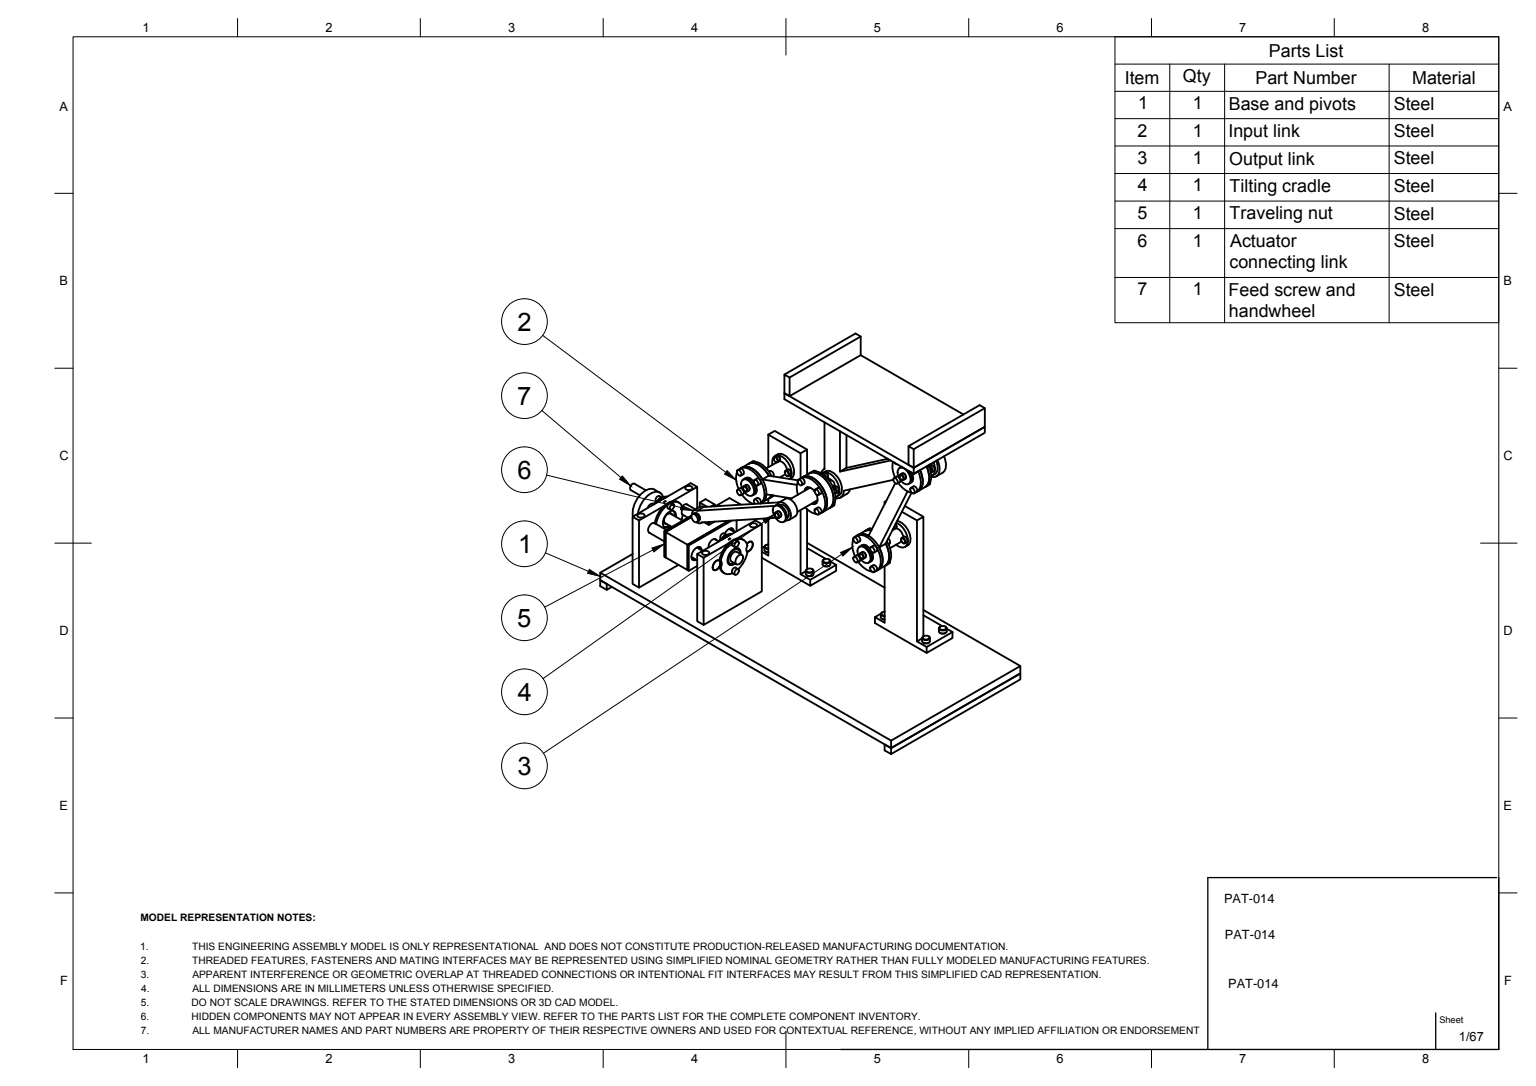
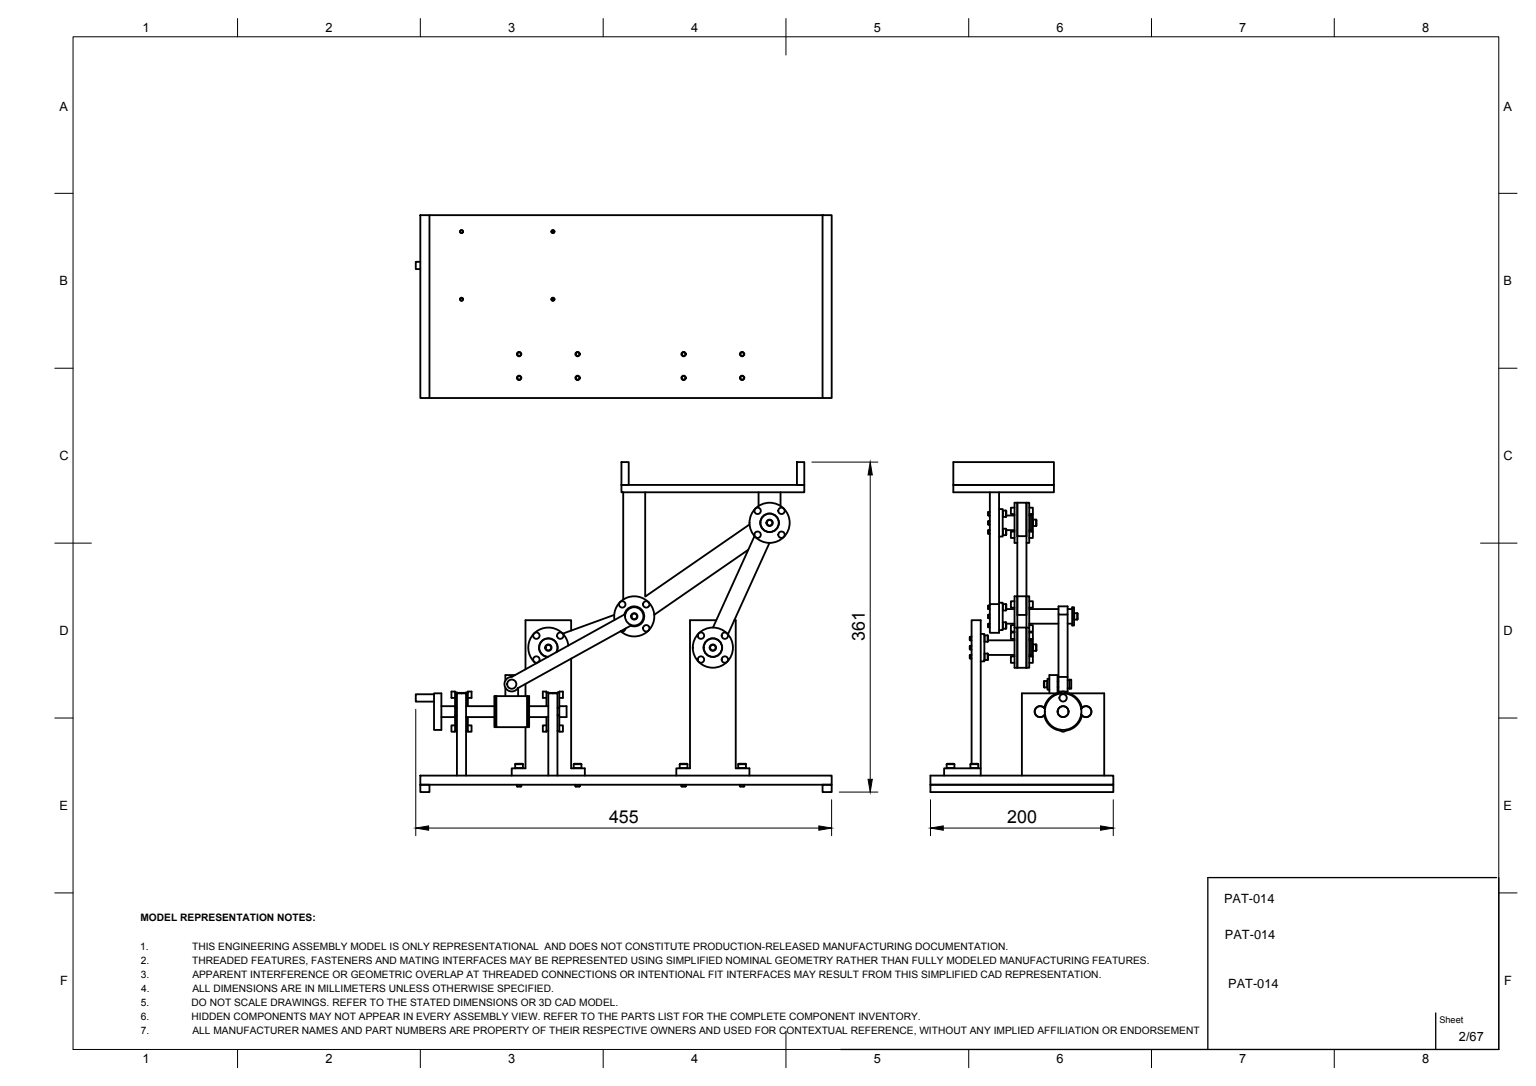
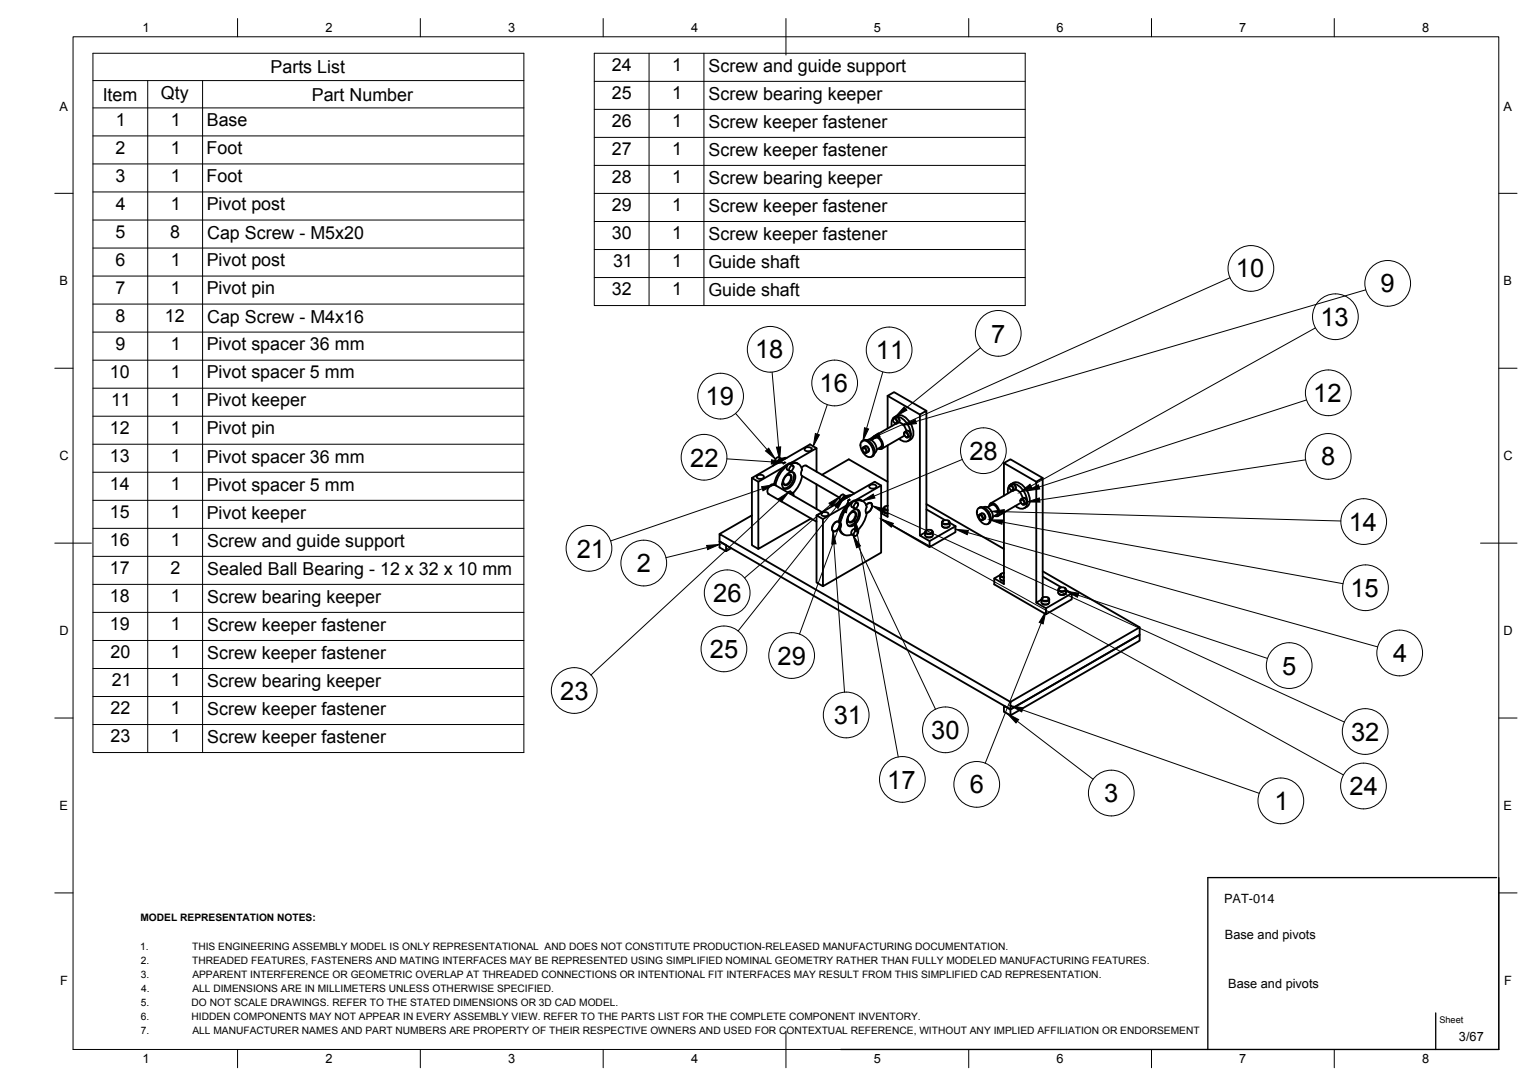
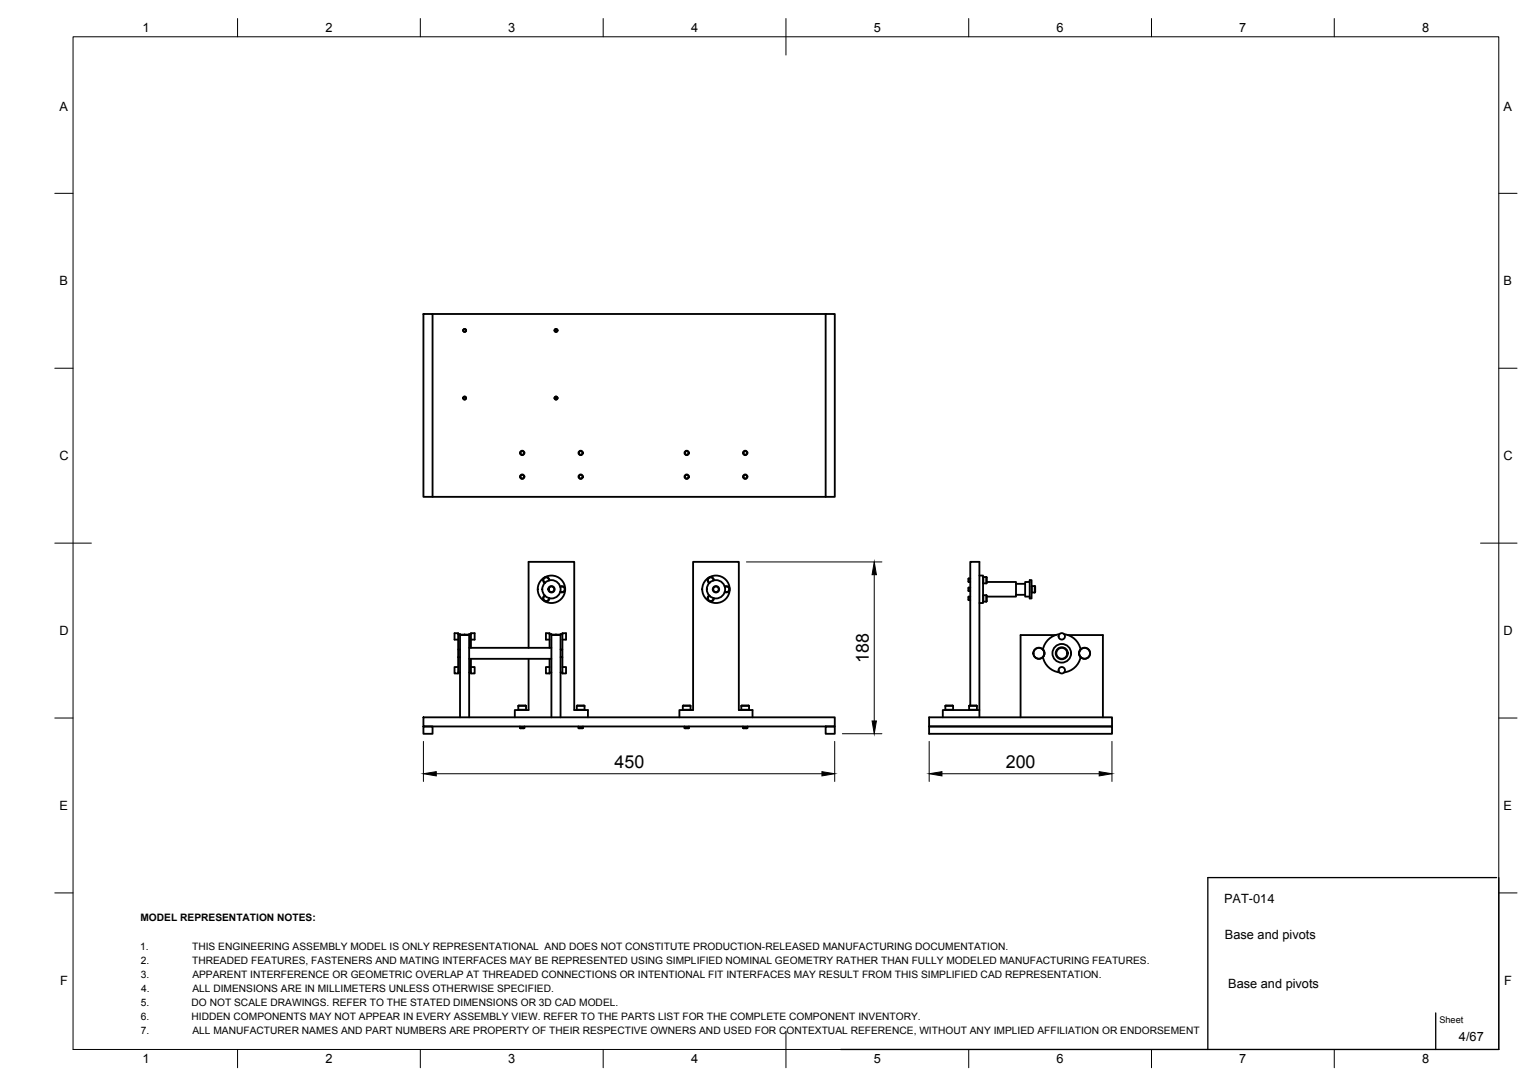
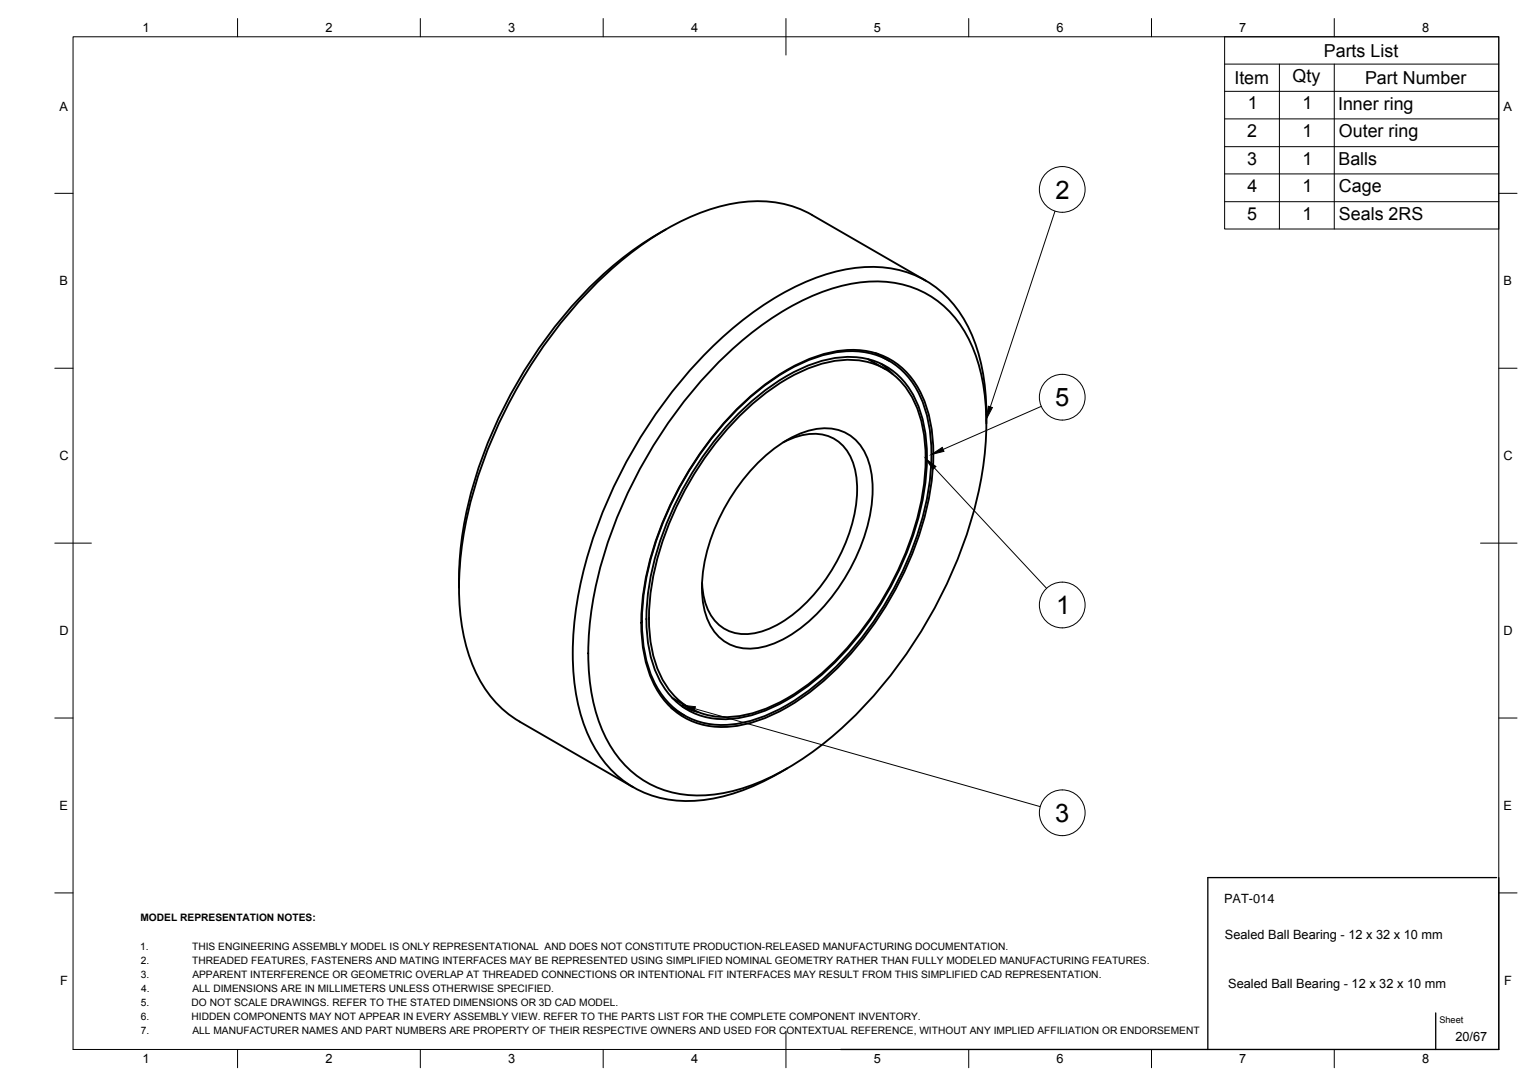
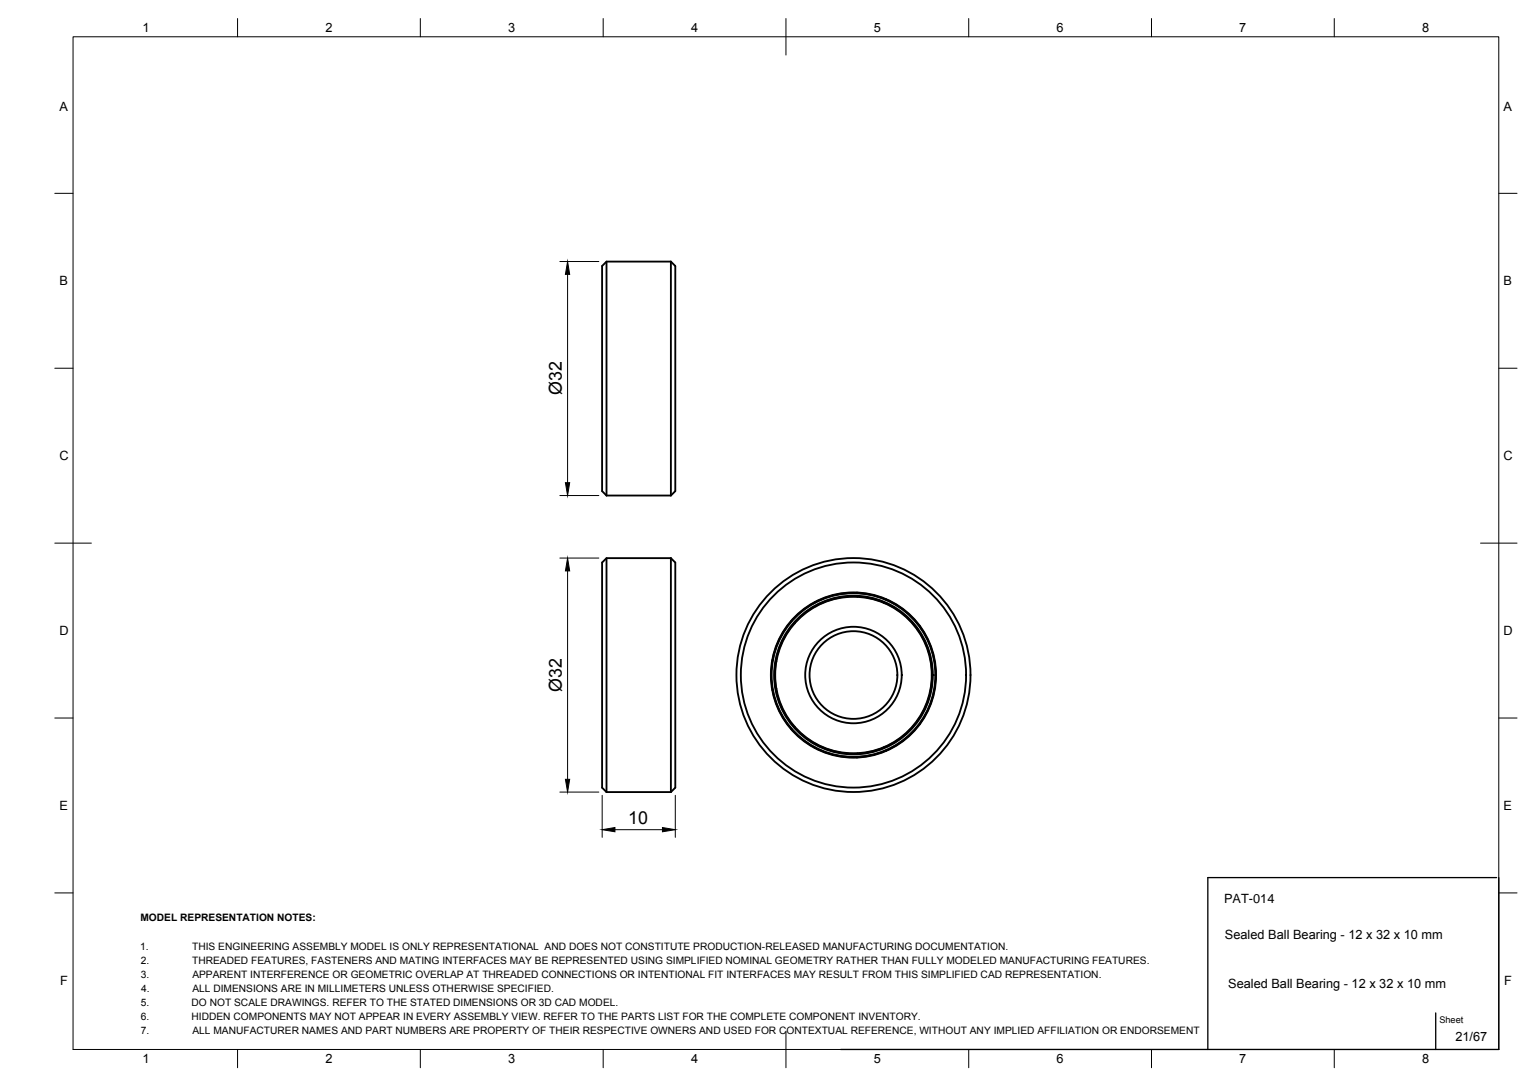
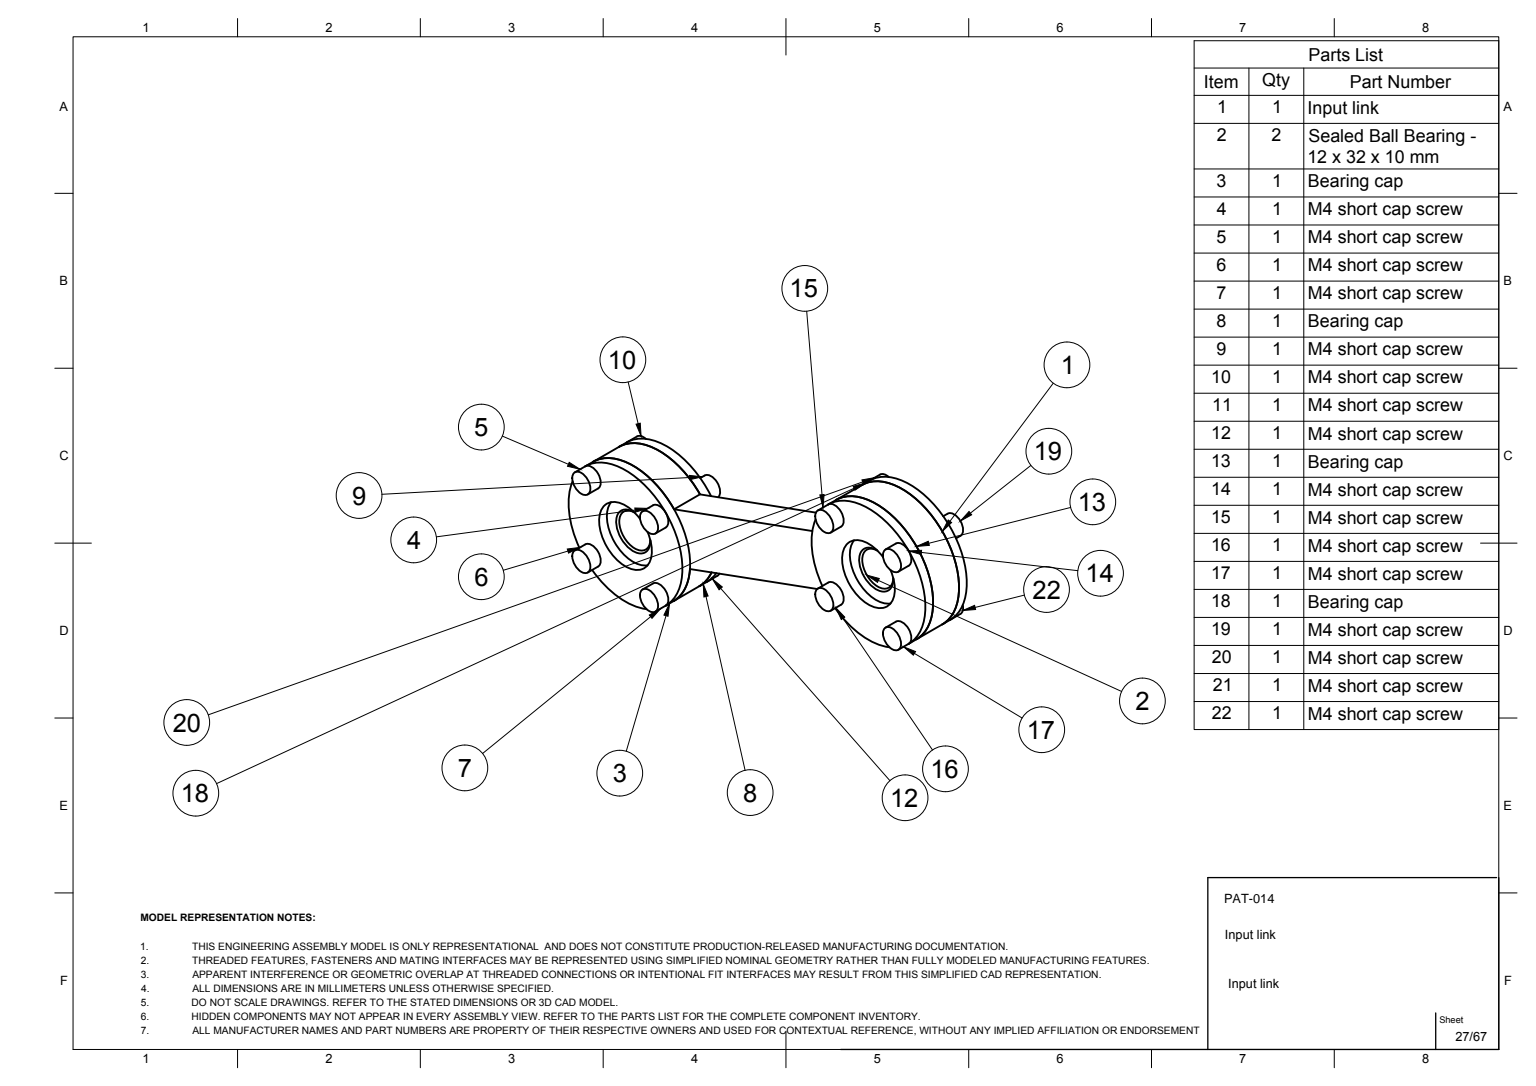
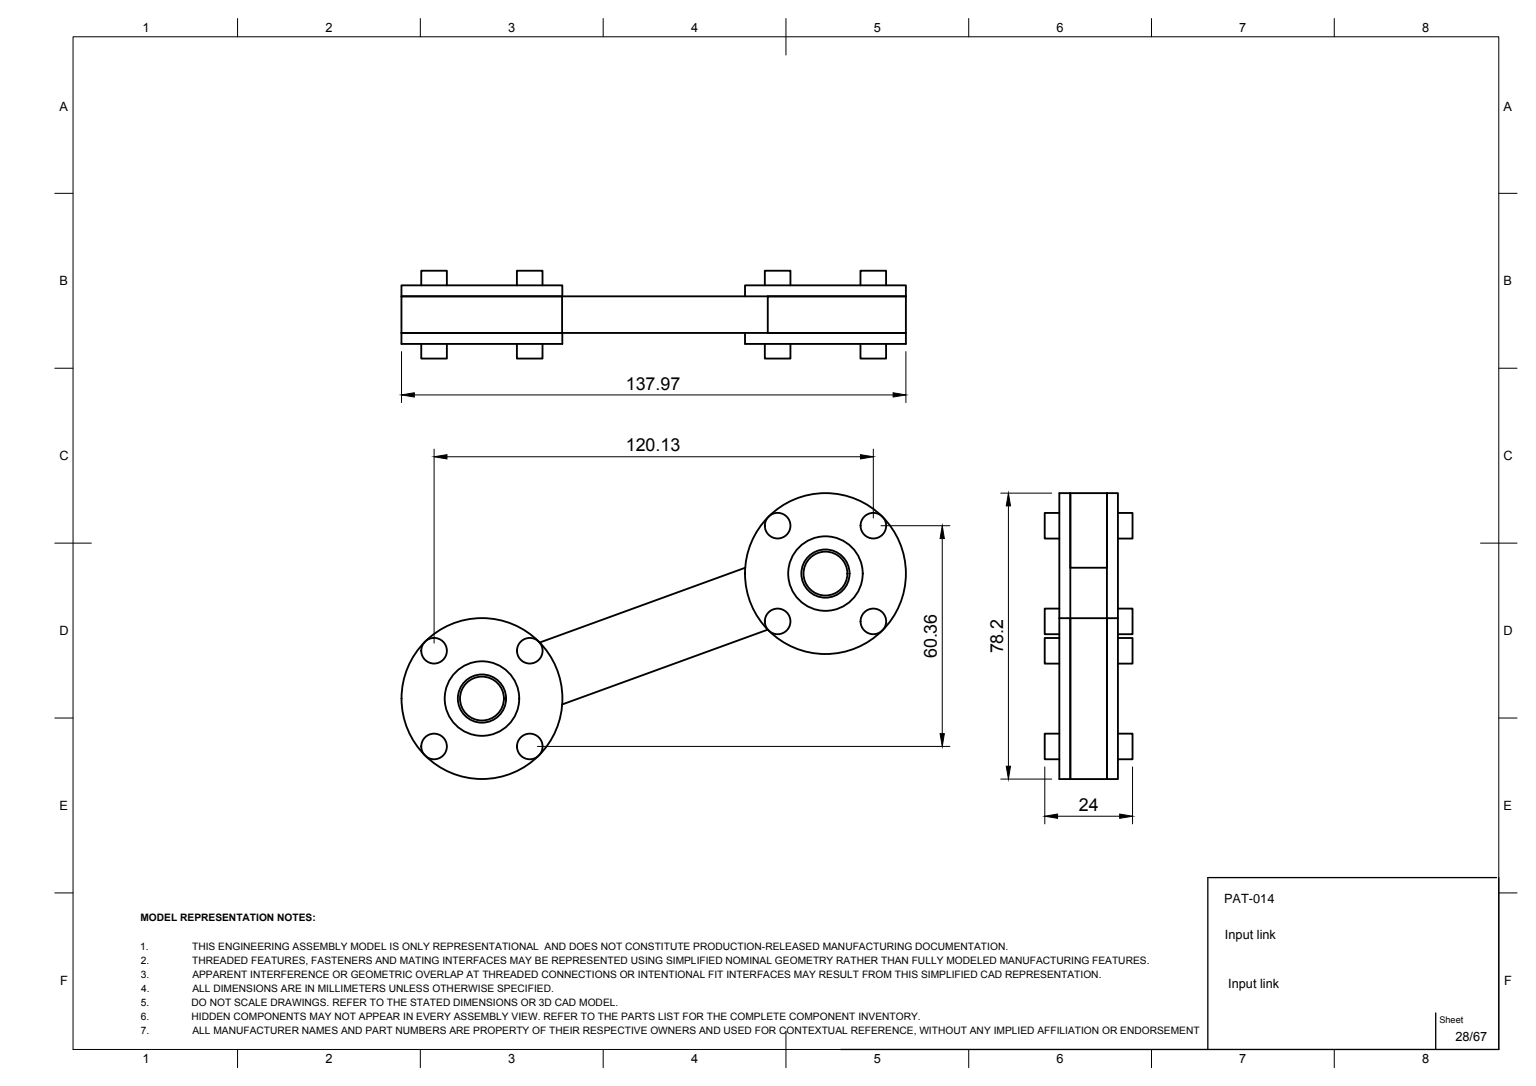
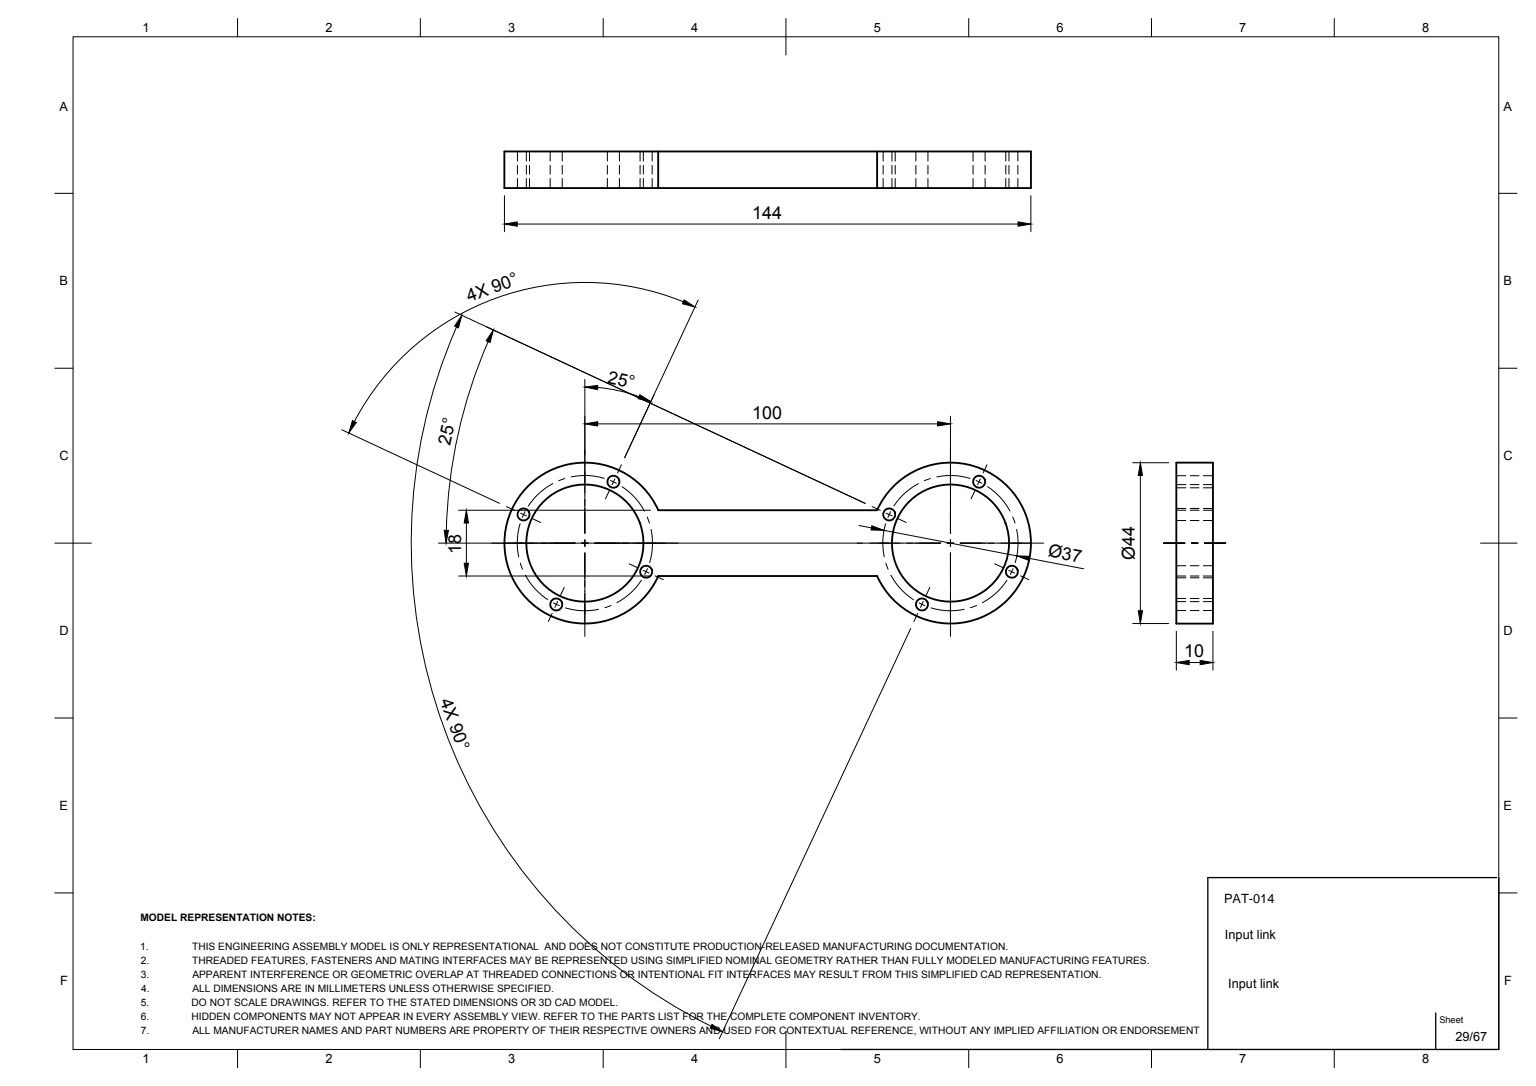
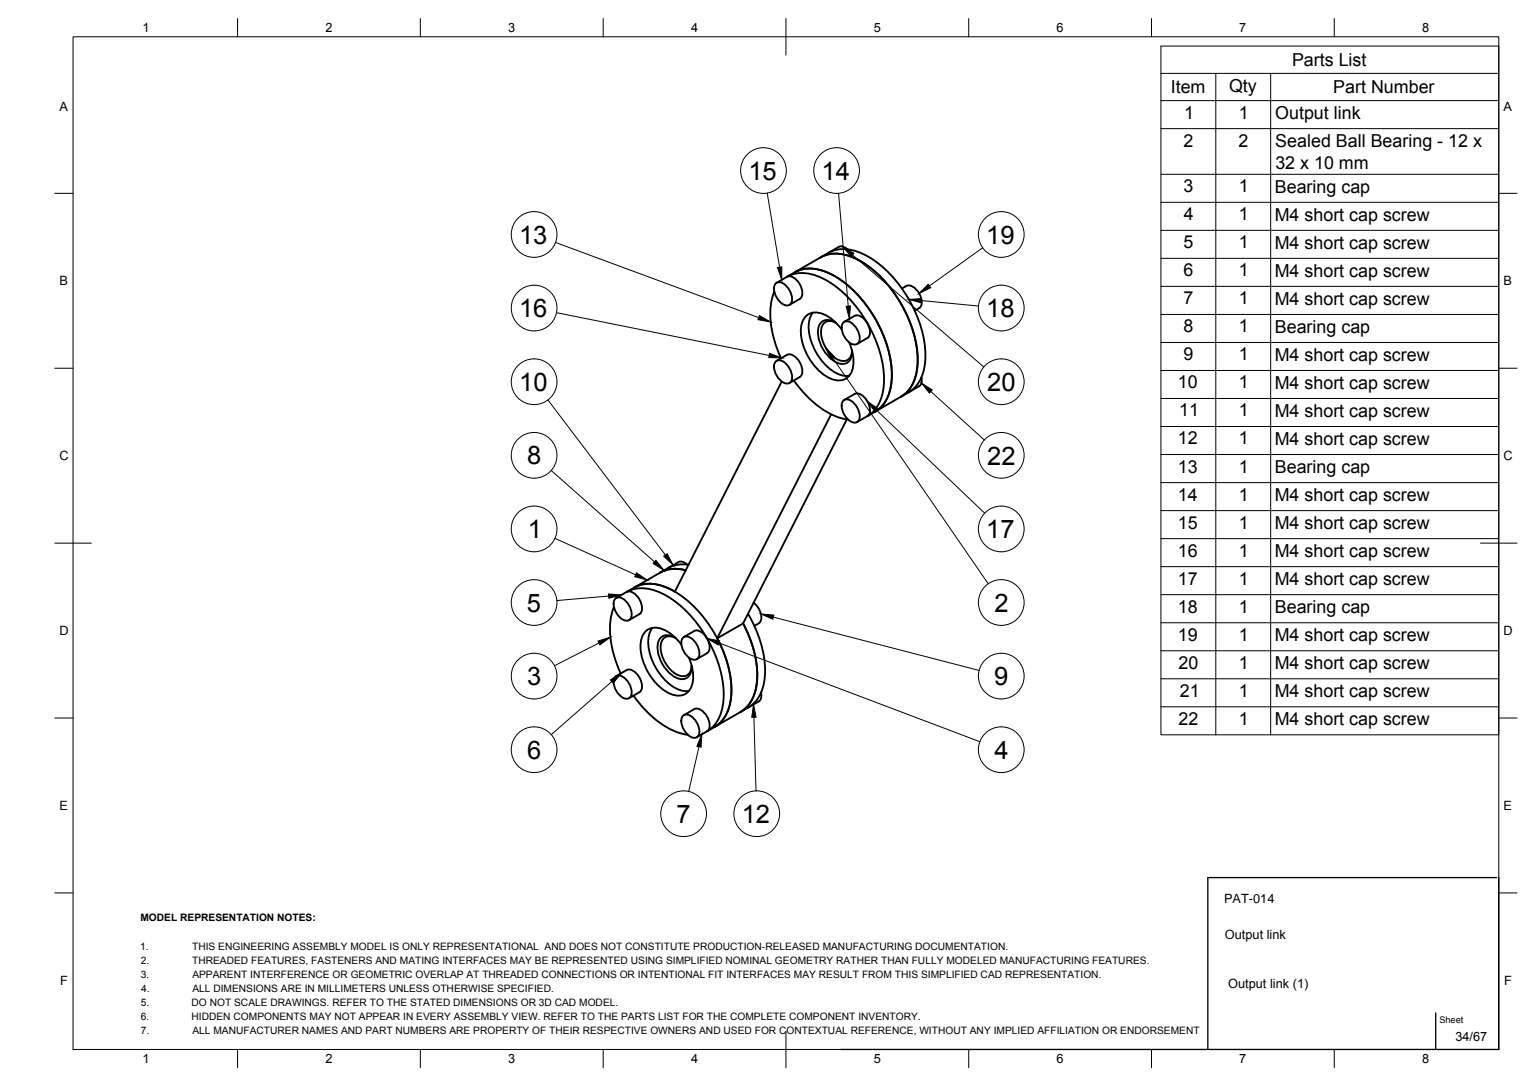
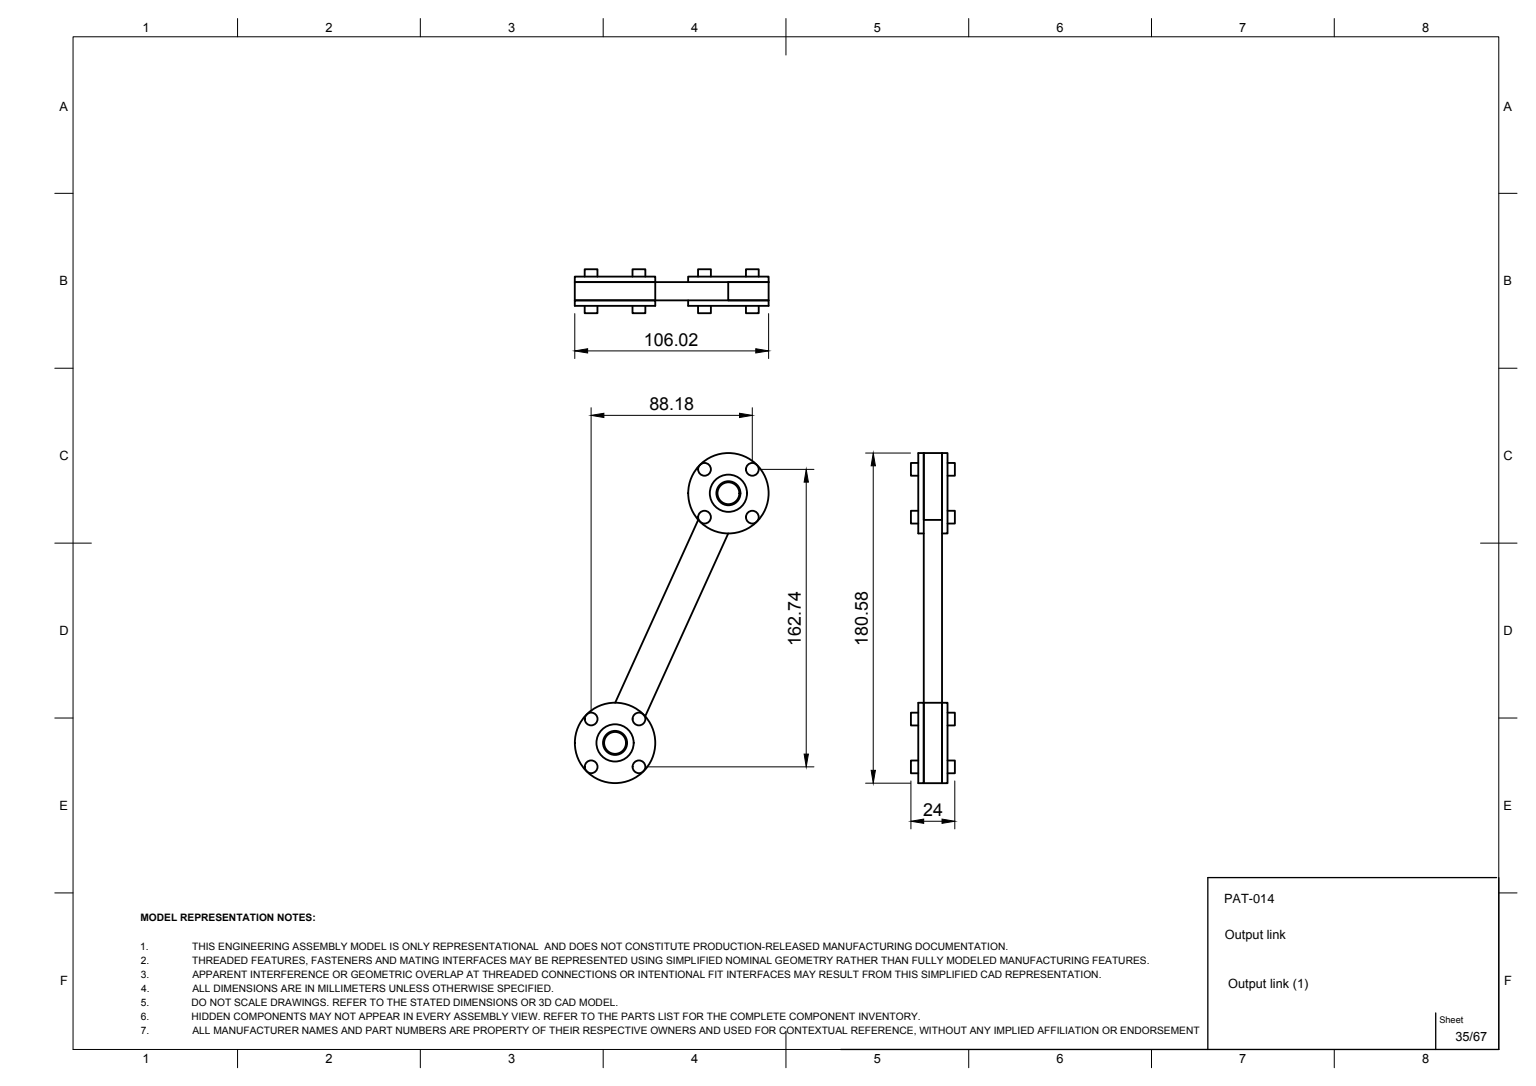
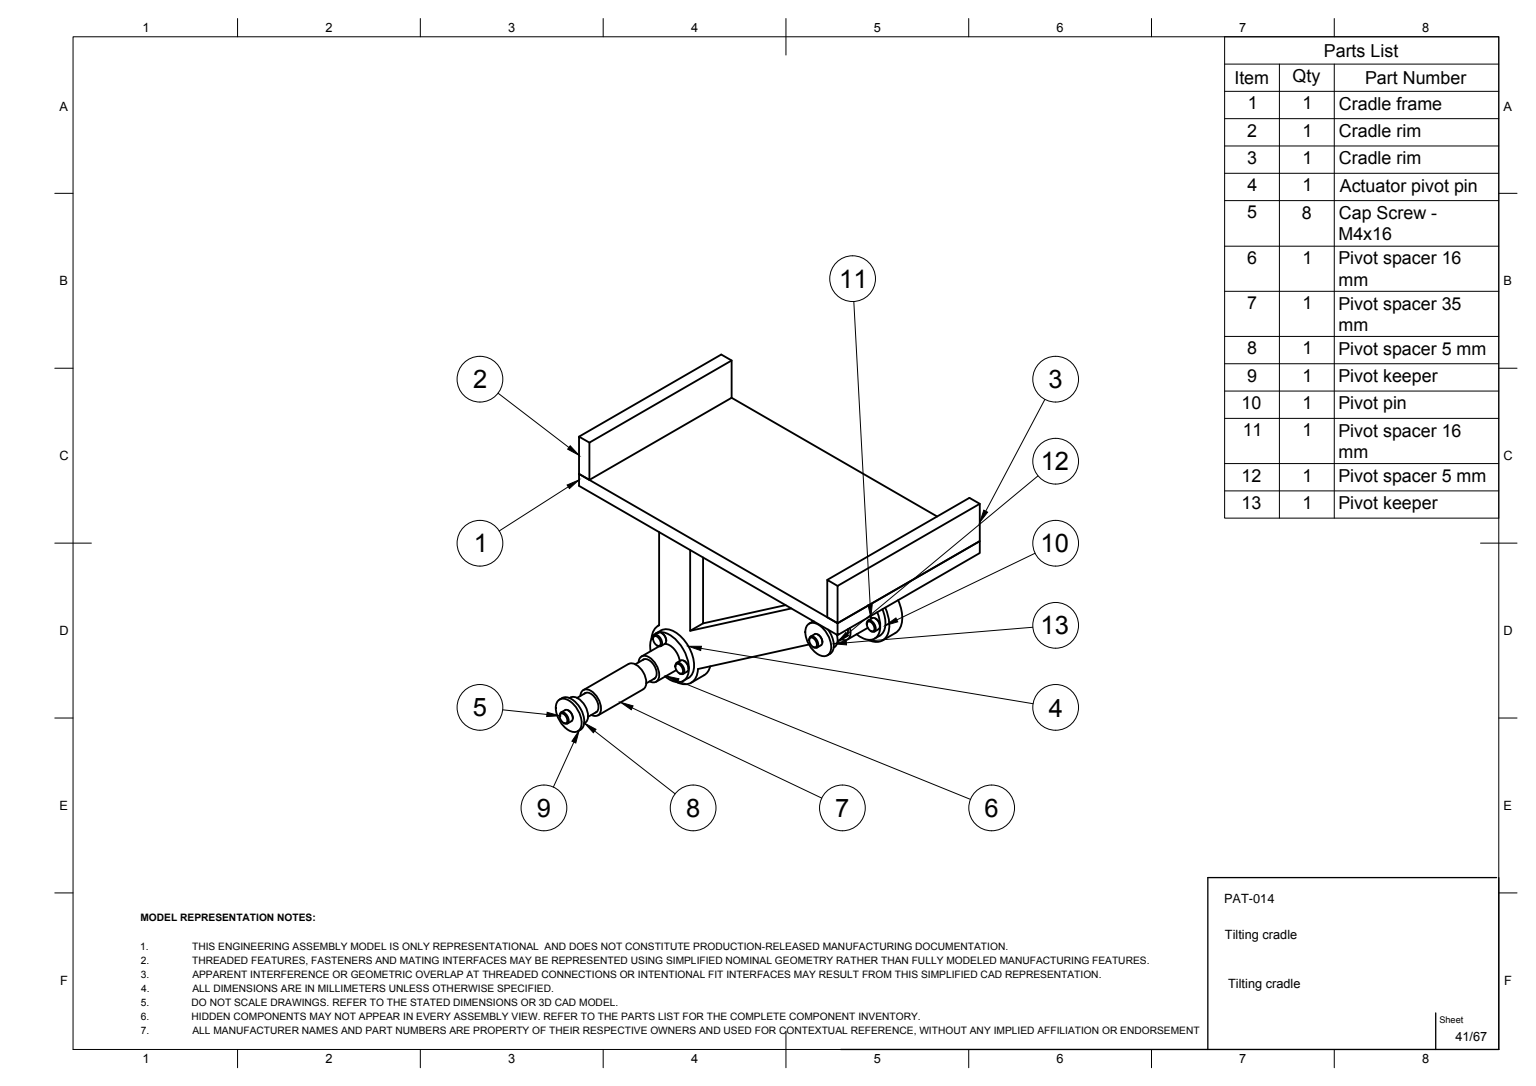
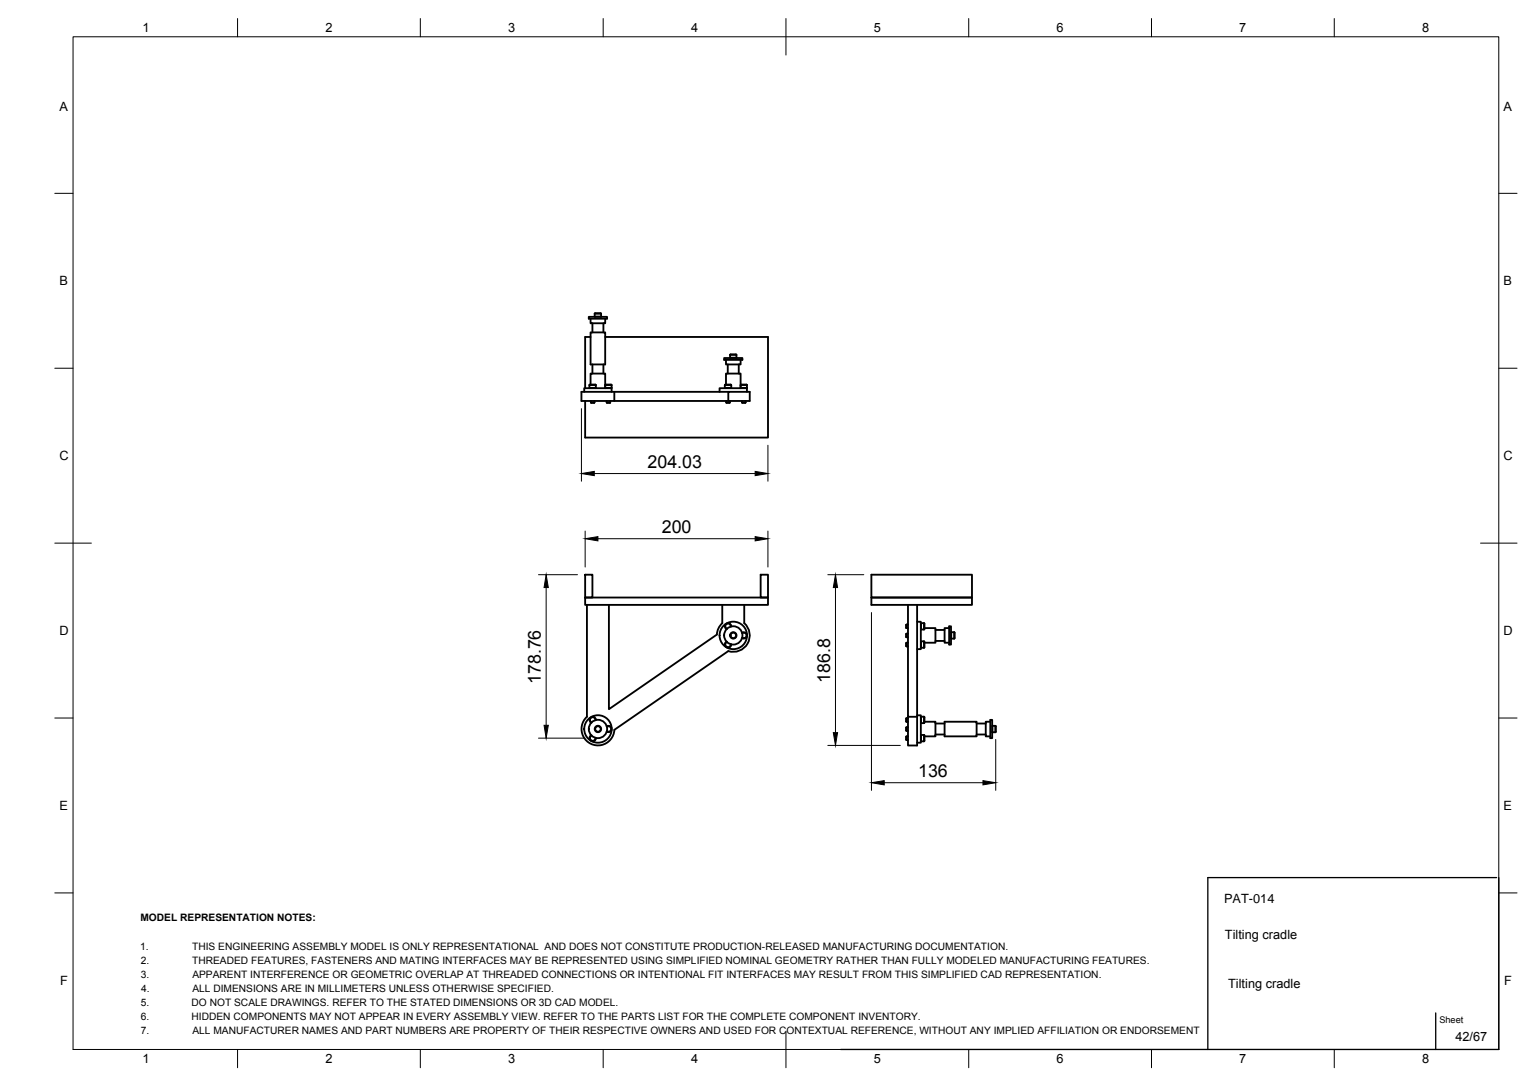
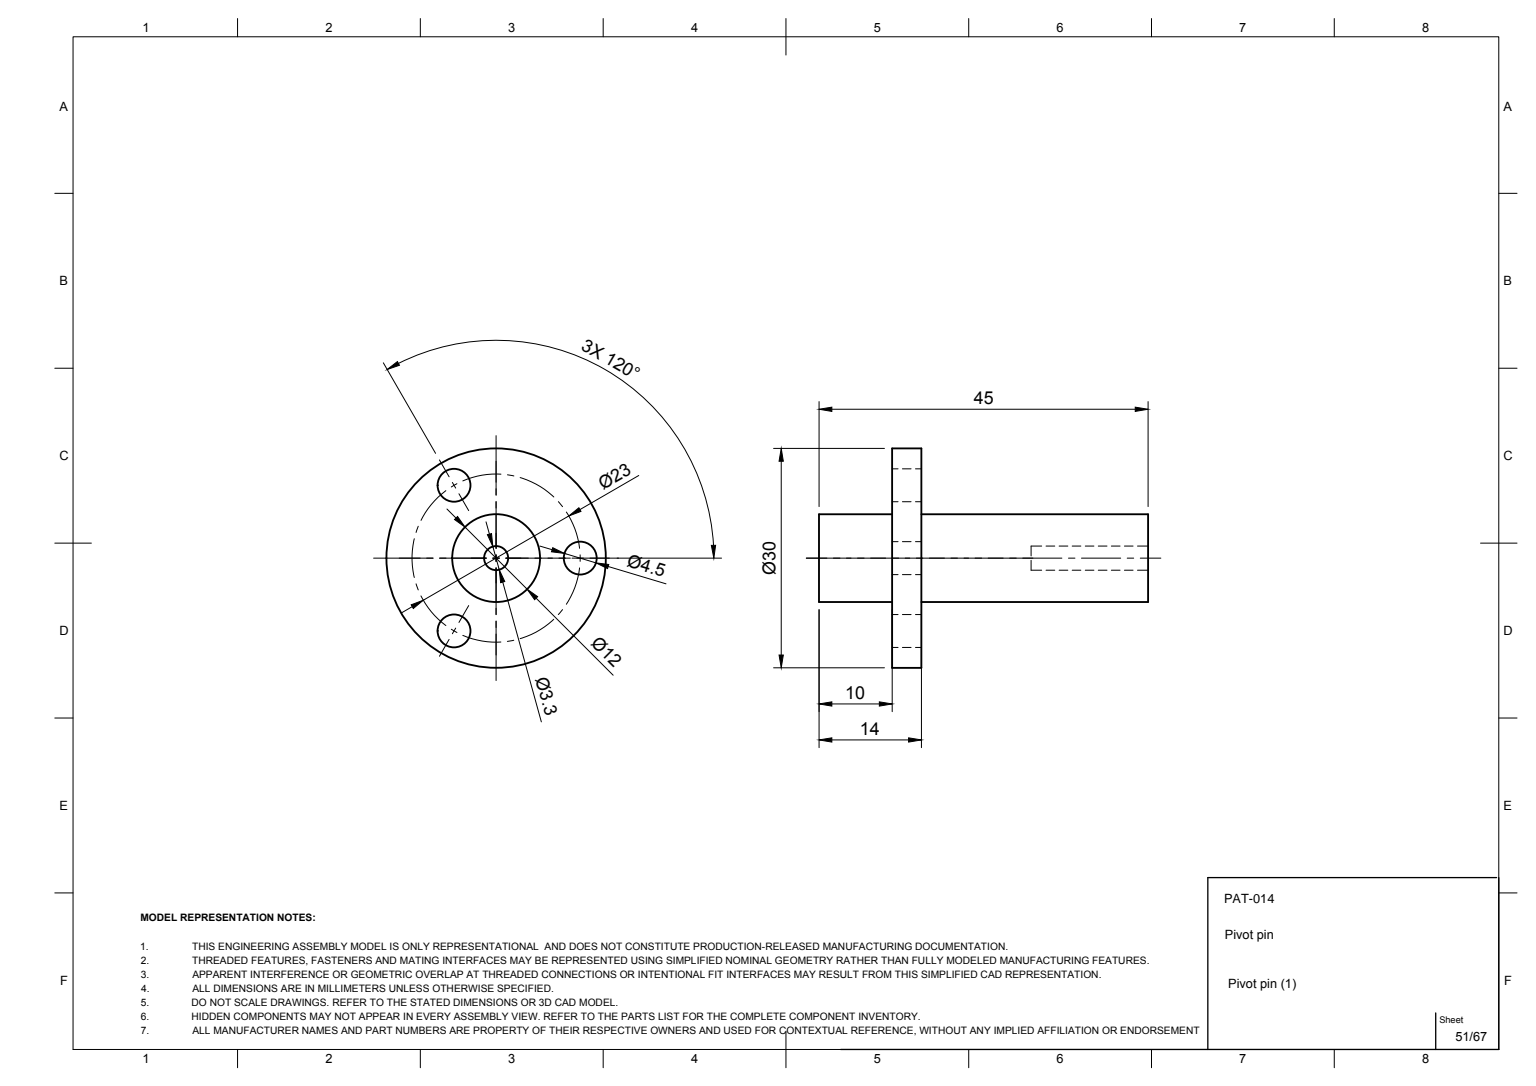
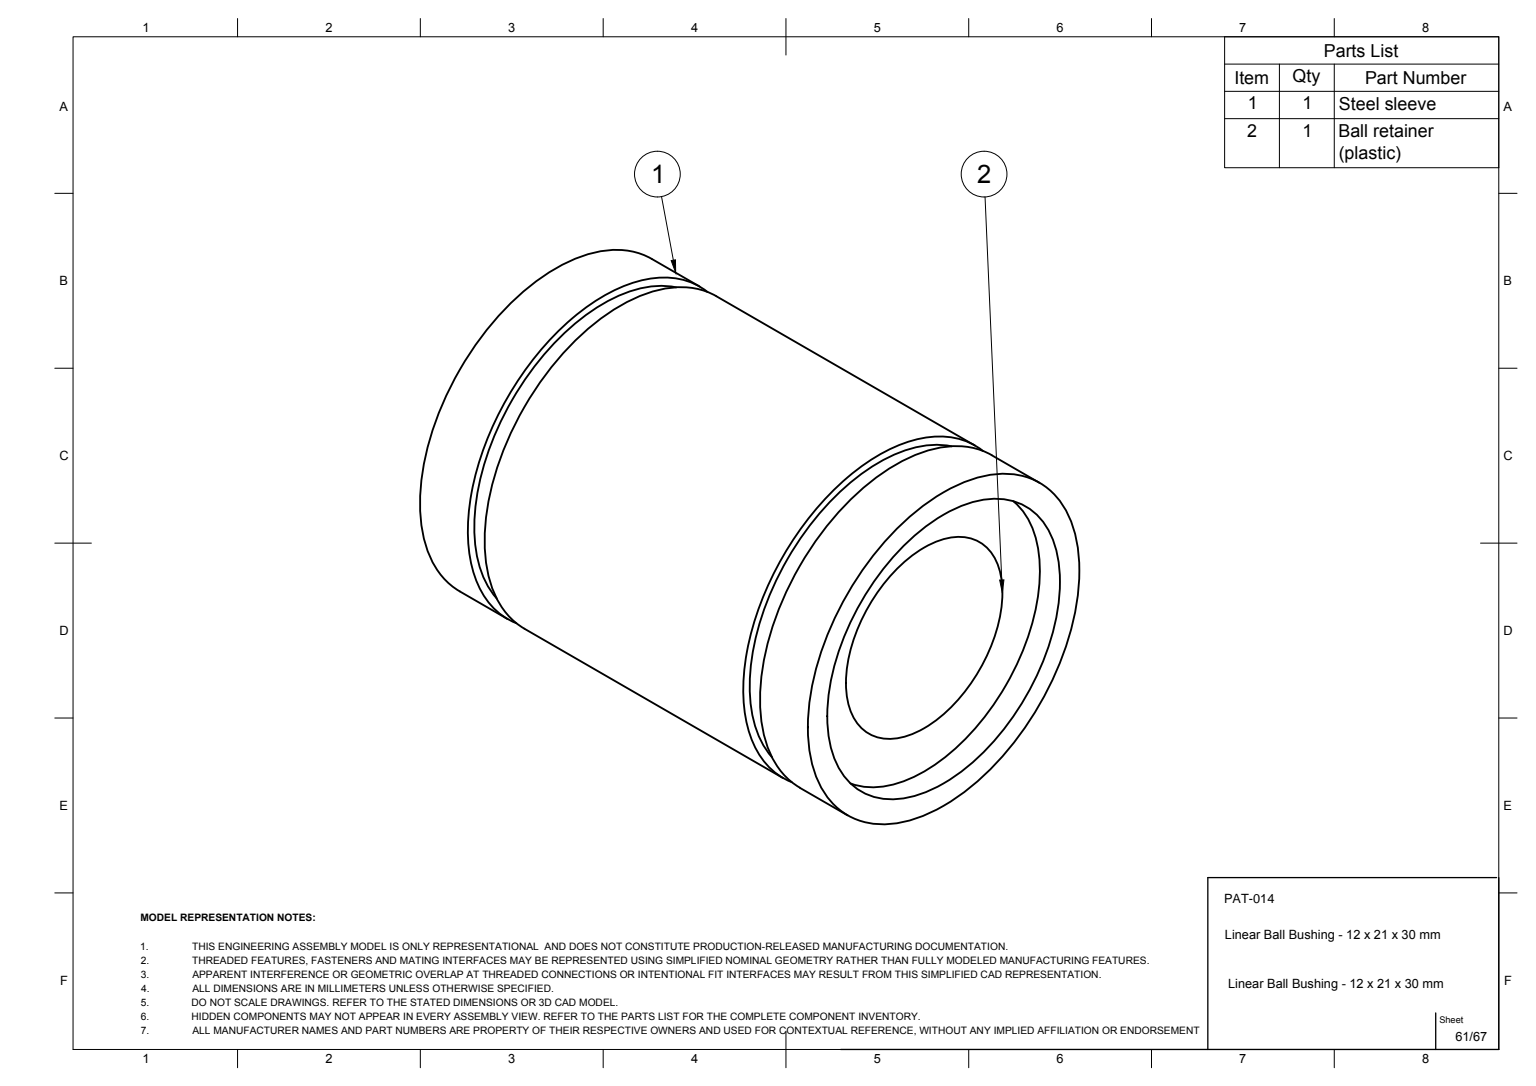
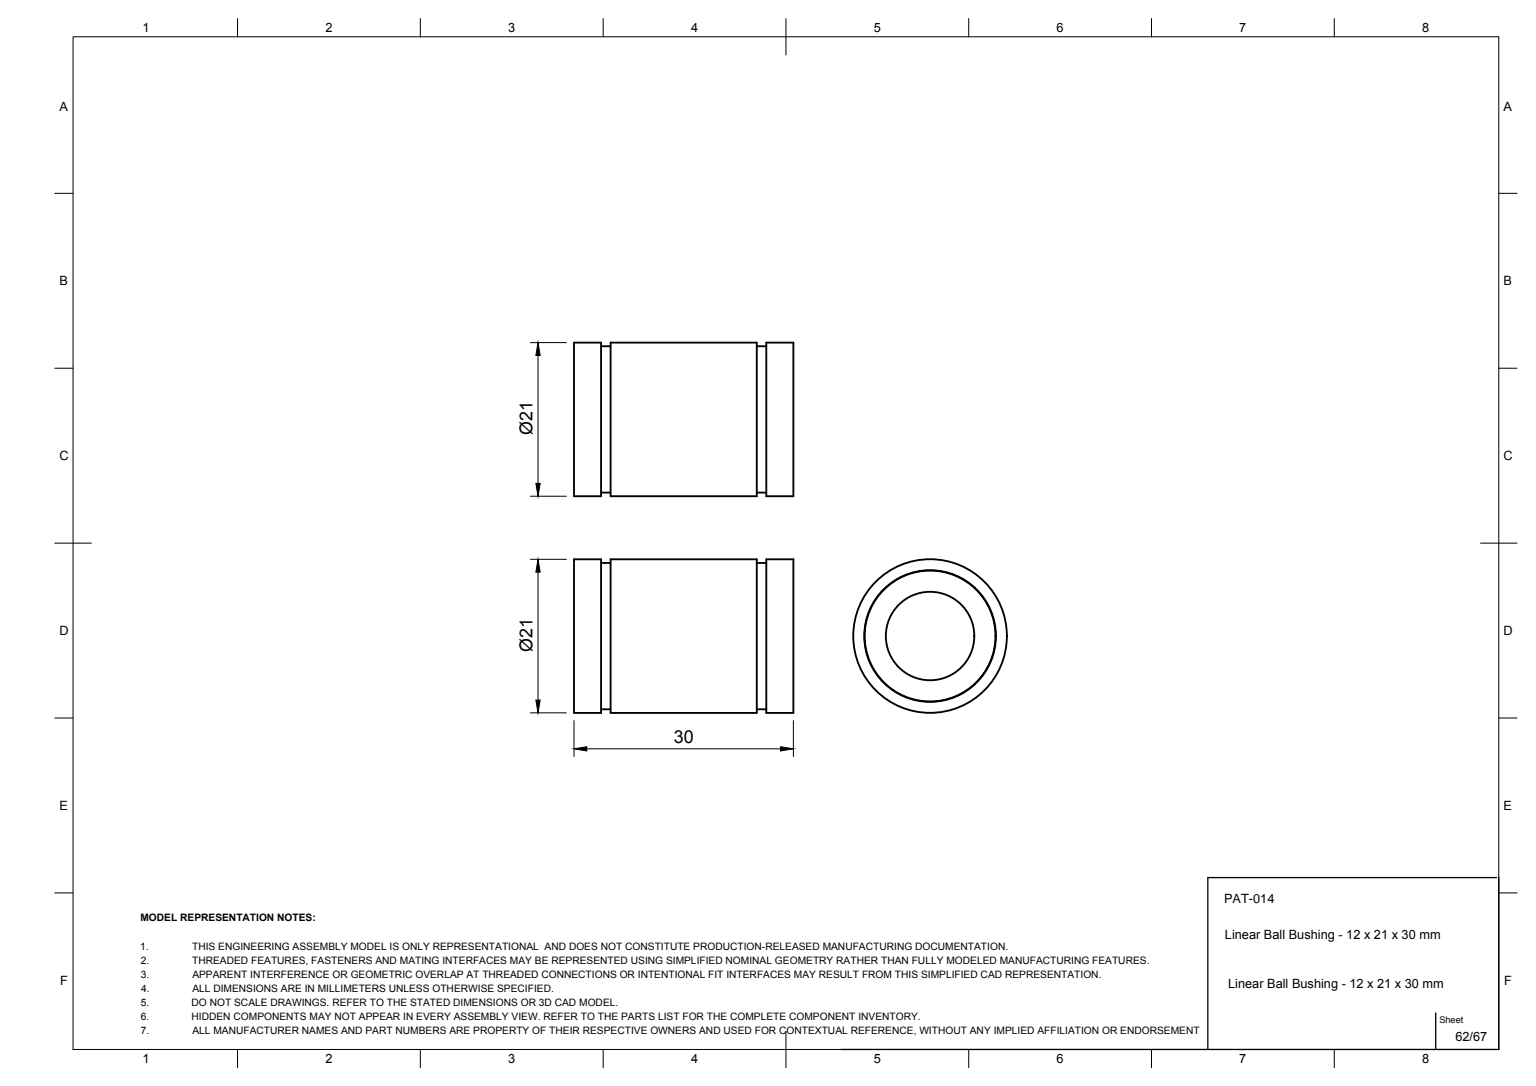
ISO-10303-21;
HEADER;
/* Generated by software containing ST-Developer
 * from STEP Tools, Inc. (www.steptools.com) 
 */

FILE_DESCRIPTION(
/* description */ ('Bin tilter linkage'),
/* implementation_level */ '2;1');

FILE_NAME(
/* name */ 'PAT-014',
/* time_stamp */ '2026-10-28T03:26:24-07:00',
/* author */ (''),
/* organization */ (''),
/* preprocessor_version */ 'ST-DEVELOPER v20.2',
/* originating_system */ 'Autodesk Translation Framework v15.17.0.0',
/* authorisation */ '');

FILE_SCHEMA (('AUTOMOTIVE_DESIGN { 1 0 10303 214 3 1 1 }'));
ENDSEC;

DATA;
#10=MECHANICAL_DESIGN_GEOMETRIC_PRESENTATION_REPRESENTATION('',(#862,#863,
#864,#865,#866,#867,#868,#869,#870,#871,#872,#873,#874,#875,#876,#877,#878,
#879,#880,#881,#882,#883,#884,#885,#886,#887,#888,#889,#890,#891,#892,#893,
#894,#895,#896,#897,#898,#899,#900,#901,#902,#903,#904,#905,#906,#907,#908,
#909,#910,#911,#912,#913,#914,#915,#916,#917,#918,#919,#920,#921,#922,#923,
#924,#925,#926,#927,#928,#929,#930,#931,#932,#933,#934,#935,#936,#937,#938,
#939,#940,#941,#942,#943,#944,#945,#946,#947,#948,#949,#950,#951,#952,#953,
#954,#955,#956,#957,#958,#959,#960,#961,#962,#963,#964,#965,#966,#967,#968,
#969,#970,#971,#972,#973,#974,#975),#23728);
#11=ITEM_DEFINED_TRANSFORMATION($,$,#14774,#14896);
#12=ITEM_DEFINED_TRANSFORMATION($,$,#14794,#14897);
#13=ITEM_DEFINED_TRANSFORMATION($,$,#14814,#14898);
#14=ITEM_DEFINED_TRANSFORMATION($,$,#14829,#14899);
#15=ITEM_DEFINED_TRANSFORMATION($,$,#14879,#14900);
#16=ITEM_DEFINED_TRANSFORMATION($,$,#14202,#14901);
#17=ITEM_DEFINED_TRANSFORMATION($,$,#14243,#14902);
#18=ITEM_DEFINED_TRANSFORMATION($,$,#14264,#14903);
#19=ITEM_DEFINED_TRANSFORMATION($,$,#14274,#14904);
#20=ITEM_DEFINED_TRANSFORMATION($,$,#14284,#14905);
#21=ITEM_DEFINED_TRANSFORMATION($,$,#14294,#14906);
#22=ITEM_DEFINED_TRANSFORMATION($,$,#14304,#14907);
#23=ITEM_DEFINED_TRANSFORMATION($,$,#14325,#14908);
#24=ITEM_DEFINED_TRANSFORMATION($,$,#14335,#14909);
#25=ITEM_DEFINED_TRANSFORMATION($,$,#14345,#14910);
#26=ITEM_DEFINED_TRANSFORMATION($,$,#14355,#14911);
#27=ITEM_DEFINED_TRANSFORMATION($,$,#14365,#14912);
#28=ITEM_DEFINED_TRANSFORMATION($,$,#14386,#14913);
#29=ITEM_DEFINED_TRANSFORMATION($,$,#14396,#14914);
#30=ITEM_DEFINED_TRANSFORMATION($,$,#14406,#14915);
#31=ITEM_DEFINED_TRANSFORMATION($,$,#14416,#14916);
#32=ITEM_DEFINED_TRANSFORMATION($,$,#14426,#14917);
#33=ITEM_DEFINED_TRANSFORMATION($,$,#14447,#14918);
#34=ITEM_DEFINED_TRANSFORMATION($,$,#14457,#14919);
#35=ITEM_DEFINED_TRANSFORMATION($,$,#14467,#14920);
#36=ITEM_DEFINED_TRANSFORMATION($,$,#14477,#14921);
#37=ITEM_DEFINED_TRANSFORMATION($,$,#14773,#14922);
#38=ITEM_DEFINED_TRANSFORMATION($,$,#14773,#14923);
#39=ITEM_DEFINED_TRANSFORMATION($,$,#14488,#14924);
#40=ITEM_DEFINED_TRANSFORMATION($,$,#14529,#14925);
#41=ITEM_DEFINED_TRANSFORMATION($,$,#14550,#14926);
#42=ITEM_DEFINED_TRANSFORMATION($,$,#14560,#14927);
#43=ITEM_DEFINED_TRANSFORMATION($,$,#14570,#14928);
#44=ITEM_DEFINED_TRANSFORMATION($,$,#14580,#14929);
#45=ITEM_DEFINED_TRANSFORMATION($,$,#14590,#14930);
#46=ITEM_DEFINED_TRANSFORMATION($,$,#14611,#14931);
#47=ITEM_DEFINED_TRANSFORMATION($,$,#14621,#14932);
#48=ITEM_DEFINED_TRANSFORMATION($,$,#14631,#14933);
#49=ITEM_DEFINED_TRANSFORMATION($,$,#14641,#14934);
#50=ITEM_DEFINED_TRANSFORMATION($,$,#14651,#14935);
#51=ITEM_DEFINED_TRANSFORMATION($,$,#14672,#14936);
#52=ITEM_DEFINED_TRANSFORMATION($,$,#14682,#14937);
#53=ITEM_DEFINED_TRANSFORMATION($,$,#14692,#14938);
#54=ITEM_DEFINED_TRANSFORMATION($,$,#14702,#14939);
#55=ITEM_DEFINED_TRANSFORMATION($,$,#14712,#14940);
#56=ITEM_DEFINED_TRANSFORMATION($,$,#14733,#14941);
#57=ITEM_DEFINED_TRANSFORMATION($,$,#14743,#14942);
#58=ITEM_DEFINED_TRANSFORMATION($,$,#14753,#14943);
#59=ITEM_DEFINED_TRANSFORMATION($,$,#14763,#14944);
#60=ITEM_DEFINED_TRANSFORMATION($,$,#14773,#14945);
#61=ITEM_DEFINED_TRANSFORMATION($,$,#14773,#14946);
#62=ITEM_DEFINED_TRANSFORMATION($,$,#13678,#15155);
#63=ITEM_DEFINED_TRANSFORMATION($,$,#13721,#15156);
#64=ITEM_DEFINED_TRANSFORMATION($,$,#13728,#15157);
#65=ITEM_DEFINED_TRANSFORMATION($,$,#13735,#15158);
#66=ITEM_DEFINED_TRANSFORMATION($,$,#13770,#15159);
#67=ITEM_DEFINED_TRANSFORMATION($,$,#13805,#15160);
#68=ITEM_DEFINED_TRANSFORMATION($,$,#13832,#15161);
#69=ITEM_DEFINED_TRANSFORMATION($,$,#13841,#15162);
#70=ITEM_DEFINED_TRANSFORMATION($,$,#13850,#15163);
#71=ITEM_DEFINED_TRANSFORMATION($,$,#13859,#15164);
#72=ITEM_DEFINED_TRANSFORMATION($,$,#13886,#15165);
#73=ITEM_DEFINED_TRANSFORMATION($,$,#13895,#15166);
#74=ITEM_DEFINED_TRANSFORMATION($,$,#13904,#15167);
#75=ITEM_DEFINED_TRANSFORMATION($,$,#13913,#15168);
#76=ITEM_DEFINED_TRANSFORMATION($,$,#13950,#15169);
#77=ITEM_DEFINED_TRANSFORMATION($,$,#13974,#15170);
#78=ITEM_DEFINED_TRANSFORMATION($,$,#13984,#15171);
#79=ITEM_DEFINED_TRANSFORMATION($,$,#13994,#15172);
#80=ITEM_DEFINED_TRANSFORMATION($,$,#14018,#15173);
#81=ITEM_DEFINED_TRANSFORMATION($,$,#14028,#15174);
#82=ITEM_DEFINED_TRANSFORMATION($,$,#14038,#15175);
#83=ITEM_DEFINED_TRANSFORMATION($,$,#14075,#15176);
#84=ITEM_DEFINED_TRANSFORMATION($,$,#14099,#15177);
#85=ITEM_DEFINED_TRANSFORMATION($,$,#14109,#15178);
#86=ITEM_DEFINED_TRANSFORMATION($,$,#14119,#15179);
#87=ITEM_DEFINED_TRANSFORMATION($,$,#14143,#15180);
#88=ITEM_DEFINED_TRANSFORMATION($,$,#14153,#15181);
#89=ITEM_DEFINED_TRANSFORMATION($,$,#14163,#15182);
#90=ITEM_DEFINED_TRANSFORMATION($,$,#14169,#15183);
#91=ITEM_DEFINED_TRANSFORMATION($,$,#14175,#15184);
#92=ITEM_DEFINED_TRANSFORMATION($,$,#14175,#15185);
#93=ITEM_DEFINED_TRANSFORMATION($,$,#14175,#15186);
#94=ITEM_DEFINED_TRANSFORMATION($,$,#14175,#15187);
#95=ITEM_DEFINED_TRANSFORMATION($,$,#14175,#15188);
#96=ITEM_DEFINED_TRANSFORMATION($,$,#14175,#15189);
#97=ITEM_DEFINED_TRANSFORMATION($,$,#14175,#15190);
#98=ITEM_DEFINED_TRANSFORMATION($,$,#14175,#15191);
#99=ITEM_DEFINED_TRANSFORMATION($,$,#15129,#15192);
#100=ITEM_DEFINED_TRANSFORMATION($,$,#15129,#15193);
#101=ITEM_DEFINED_TRANSFORMATION($,$,#15129,#15194);
#102=ITEM_DEFINED_TRANSFORMATION($,$,#15129,#15195);
#103=ITEM_DEFINED_TRANSFORMATION($,$,#15129,#15196);
#104=ITEM_DEFINED_TRANSFORMATION($,$,#15129,#15197);
#105=ITEM_DEFINED_TRANSFORMATION($,$,#15129,#15198);
#106=ITEM_DEFINED_TRANSFORMATION($,$,#15129,#15199);
#107=ITEM_DEFINED_TRANSFORMATION($,$,#14773,#15200);
#108=ITEM_DEFINED_TRANSFORMATION($,$,#15129,#15201);
#109=ITEM_DEFINED_TRANSFORMATION($,$,#15129,#15202);
#110=ITEM_DEFINED_TRANSFORMATION($,$,#14773,#15203);
#111=ITEM_DEFINED_TRANSFORMATION($,$,#15129,#15204);
#112=ITEM_DEFINED_TRANSFORMATION($,$,#15129,#15205);
#113=ITEM_DEFINED_TRANSFORMATION($,$,#14948,#15206);
#114=ITEM_DEFINED_TRANSFORMATION($,$,#14998,#15207);
#115=ITEM_DEFINED_TRANSFORMATION($,$,#15005,#15208);
#116=ITEM_DEFINED_TRANSFORMATION($,$,#15012,#15209);
#117=ITEM_DEFINED_TRANSFORMATION($,$,#15039,#15210);
#118=ITEM_DEFINED_TRANSFORMATION($,$,#15048,#15211);
#119=ITEM_DEFINED_TRANSFORMATION($,$,#15057,#15212);
#120=ITEM_DEFINED_TRANSFORMATION($,$,#15066,#15213);
#121=ITEM_DEFINED_TRANSFORMATION($,$,#15075,#15214);
#122=ITEM_DEFINED_TRANSFORMATION($,$,#15102,#15215);
#123=ITEM_DEFINED_TRANSFORMATION($,$,#15111,#15216);
#124=ITEM_DEFINED_TRANSFORMATION($,$,#15120,#15217);
#125=ITEM_DEFINED_TRANSFORMATION($,$,#15129,#15218);
#126=ITEM_DEFINED_TRANSFORMATION($,$,#15129,#15219);
#127=ITEM_DEFINED_TRANSFORMATION($,$,#15129,#15220);
#128=ITEM_DEFINED_TRANSFORMATION($,$,#15129,#15221);
#129=ITEM_DEFINED_TRANSFORMATION($,$,#15129,#15222);
#130=ITEM_DEFINED_TRANSFORMATION($,$,#15129,#15223);
#131=ITEM_DEFINED_TRANSFORMATION($,$,#15129,#15224);
#132=ITEM_DEFINED_TRANSFORMATION($,$,#15129,#15225);
#133=ITEM_DEFINED_TRANSFORMATION($,$,#15318,#15367);
#134=ITEM_DEFINED_TRANSFORMATION($,$,#15350,#15368);
#135=ITEM_DEFINED_TRANSFORMATION($,$,#15227,#15393);
#136=ITEM_DEFINED_TRANSFORMATION($,$,#15243,#15394);
#137=ITEM_DEFINED_TRANSFORMATION($,$,#15259,#15395);
#138=ITEM_DEFINED_TRANSFORMATION($,$,#15275,#15396);
#139=ITEM_DEFINED_TRANSFORMATION($,$,#15285,#15397);
#140=ITEM_DEFINED_TRANSFORMATION($,$,#15299,#15398);
#141=ITEM_DEFINED_TRANSFORMATION($,$,#15308,#15399);
#142=ITEM_DEFINED_TRANSFORMATION($,$,#15317,#15400);
#143=ITEM_DEFINED_TRANSFORMATION($,$,#15317,#15401);
#144=ITEM_DEFINED_TRANSFORMATION($,$,#15369,#15402);
#145=ITEM_DEFINED_TRANSFORMATION($,$,#15404,#15421);
#146=ITEM_DEFINED_TRANSFORMATION($,$,#15423,#15462);
#147=ITEM_DEFINED_TRANSFORMATION($,$,#15429,#15463);
#148=ITEM_DEFINED_TRANSFORMATION($,$,#15438,#15464);
#149=ITEM_DEFINED_TRANSFORMATION($,$,#15447,#15465);
#150=ITEM_DEFINED_TRANSFORMATION($,$,#15456,#15466);
#151=ITEM_DEFINED_TRANSFORMATION($,$,#13677,#15467);
#152=ITEM_DEFINED_TRANSFORMATION($,$,#14201,#15468);
#153=ITEM_DEFINED_TRANSFORMATION($,$,#14487,#15469);
#154=ITEM_DEFINED_TRANSFORMATION($,$,#14947,#15470);
#155=ITEM_DEFINED_TRANSFORMATION($,$,#15226,#15471);
#156=ITEM_DEFINED_TRANSFORMATION($,$,#15403,#15472);
#157=ITEM_DEFINED_TRANSFORMATION($,$,#15422,#15473);
#158=(
REPRESENTATION_RELATIONSHIP($,$,#24189,#24188)
REPRESENTATION_RELATIONSHIP_WITH_TRANSFORMATION(#11)
SHAPE_REPRESENTATION_RELATIONSHIP()
);
#159=(
REPRESENTATION_RELATIONSHIP($,$,#24190,#24188)
REPRESENTATION_RELATIONSHIP_WITH_TRANSFORMATION(#12)
SHAPE_REPRESENTATION_RELATIONSHIP()
);
#160=(
REPRESENTATION_RELATIONSHIP($,$,#24191,#24188)
REPRESENTATION_RELATIONSHIP_WITH_TRANSFORMATION(#13)
SHAPE_REPRESENTATION_RELATIONSHIP()
);
#161=(
REPRESENTATION_RELATIONSHIP($,$,#24192,#24188)
REPRESENTATION_RELATIONSHIP_WITH_TRANSFORMATION(#14)
SHAPE_REPRESENTATION_RELATIONSHIP()
);
#162=(
REPRESENTATION_RELATIONSHIP($,$,#24193,#24188)
REPRESENTATION_RELATIONSHIP_WITH_TRANSFORMATION(#15)
SHAPE_REPRESENTATION_RELATIONSHIP()
);
#163=(
REPRESENTATION_RELATIONSHIP($,$,#24145,#24144)
REPRESENTATION_RELATIONSHIP_WITH_TRANSFORMATION(#16)
SHAPE_REPRESENTATION_RELATIONSHIP()
);
#164=(
REPRESENTATION_RELATIONSHIP($,$,#24146,#24144)
REPRESENTATION_RELATIONSHIP_WITH_TRANSFORMATION(#17)
SHAPE_REPRESENTATION_RELATIONSHIP()
);
#165=(
REPRESENTATION_RELATIONSHIP($,$,#24147,#24144)
REPRESENTATION_RELATIONSHIP_WITH_TRANSFORMATION(#18)
SHAPE_REPRESENTATION_RELATIONSHIP()
);
#166=(
REPRESENTATION_RELATIONSHIP($,$,#24148,#24144)
REPRESENTATION_RELATIONSHIP_WITH_TRANSFORMATION(#19)
SHAPE_REPRESENTATION_RELATIONSHIP()
);
#167=(
REPRESENTATION_RELATIONSHIP($,$,#24149,#24144)
REPRESENTATION_RELATIONSHIP_WITH_TRANSFORMATION(#20)
SHAPE_REPRESENTATION_RELATIONSHIP()
);
#168=(
REPRESENTATION_RELATIONSHIP($,$,#24150,#24144)
REPRESENTATION_RELATIONSHIP_WITH_TRANSFORMATION(#21)
SHAPE_REPRESENTATION_RELATIONSHIP()
);
#169=(
REPRESENTATION_RELATIONSHIP($,$,#24151,#24144)
REPRESENTATION_RELATIONSHIP_WITH_TRANSFORMATION(#22)
SHAPE_REPRESENTATION_RELATIONSHIP()
);
#170=(
REPRESENTATION_RELATIONSHIP($,$,#24152,#24144)
REPRESENTATION_RELATIONSHIP_WITH_TRANSFORMATION(#23)
SHAPE_REPRESENTATION_RELATIONSHIP()
);
#171=(
REPRESENTATION_RELATIONSHIP($,$,#24153,#24144)
REPRESENTATION_RELATIONSHIP_WITH_TRANSFORMATION(#24)
SHAPE_REPRESENTATION_RELATIONSHIP()
);
#172=(
REPRESENTATION_RELATIONSHIP($,$,#24154,#24144)
REPRESENTATION_RELATIONSHIP_WITH_TRANSFORMATION(#25)
SHAPE_REPRESENTATION_RELATIONSHIP()
);
#173=(
REPRESENTATION_RELATIONSHIP($,$,#24155,#24144)
REPRESENTATION_RELATIONSHIP_WITH_TRANSFORMATION(#26)
SHAPE_REPRESENTATION_RELATIONSHIP()
);
#174=(
REPRESENTATION_RELATIONSHIP($,$,#24156,#24144)
REPRESENTATION_RELATIONSHIP_WITH_TRANSFORMATION(#27)
SHAPE_REPRESENTATION_RELATIONSHIP()
);
#175=(
REPRESENTATION_RELATIONSHIP($,$,#24157,#24144)
REPRESENTATION_RELATIONSHIP_WITH_TRANSFORMATION(#28)
SHAPE_REPRESENTATION_RELATIONSHIP()
);
#176=(
REPRESENTATION_RELATIONSHIP($,$,#24158,#24144)
REPRESENTATION_RELATIONSHIP_WITH_TRANSFORMATION(#29)
SHAPE_REPRESENTATION_RELATIONSHIP()
);
#177=(
REPRESENTATION_RELATIONSHIP($,$,#24159,#24144)
REPRESENTATION_RELATIONSHIP_WITH_TRANSFORMATION(#30)
SHAPE_REPRESENTATION_RELATIONSHIP()
);
#178=(
REPRESENTATION_RELATIONSHIP($,$,#24160,#24144)
REPRESENTATION_RELATIONSHIP_WITH_TRANSFORMATION(#31)
SHAPE_REPRESENTATION_RELATIONSHIP()
);
#179=(
REPRESENTATION_RELATIONSHIP($,$,#24161,#24144)
REPRESENTATION_RELATIONSHIP_WITH_TRANSFORMATION(#32)
SHAPE_REPRESENTATION_RELATIONSHIP()
);
#180=(
REPRESENTATION_RELATIONSHIP($,$,#24162,#24144)
REPRESENTATION_RELATIONSHIP_WITH_TRANSFORMATION(#33)
SHAPE_REPRESENTATION_RELATIONSHIP()
);
#181=(
REPRESENTATION_RELATIONSHIP($,$,#24163,#24144)
REPRESENTATION_RELATIONSHIP_WITH_TRANSFORMATION(#34)
SHAPE_REPRESENTATION_RELATIONSHIP()
);
#182=(
REPRESENTATION_RELATIONSHIP($,$,#24164,#24144)
REPRESENTATION_RELATIONSHIP_WITH_TRANSFORMATION(#35)
SHAPE_REPRESENTATION_RELATIONSHIP()
);
#183=(
REPRESENTATION_RELATIONSHIP($,$,#24165,#24144)
REPRESENTATION_RELATIONSHIP_WITH_TRANSFORMATION(#36)
SHAPE_REPRESENTATION_RELATIONSHIP()
);
#184=(
REPRESENTATION_RELATIONSHIP($,$,#24188,#24144)
REPRESENTATION_RELATIONSHIP_WITH_TRANSFORMATION(#37)
SHAPE_REPRESENTATION_RELATIONSHIP()
);
#185=(
REPRESENTATION_RELATIONSHIP($,$,#24188,#24144)
REPRESENTATION_RELATIONSHIP_WITH_TRANSFORMATION(#38)
SHAPE_REPRESENTATION_RELATIONSHIP()
);
#186=(
REPRESENTATION_RELATIONSHIP($,$,#24167,#24166)
REPRESENTATION_RELATIONSHIP_WITH_TRANSFORMATION(#39)
SHAPE_REPRESENTATION_RELATIONSHIP()
);
#187=(
REPRESENTATION_RELATIONSHIP($,$,#24168,#24166)
REPRESENTATION_RELATIONSHIP_WITH_TRANSFORMATION(#40)
SHAPE_REPRESENTATION_RELATIONSHIP()
);
#188=(
REPRESENTATION_RELATIONSHIP($,$,#24169,#24166)
REPRESENTATION_RELATIONSHIP_WITH_TRANSFORMATION(#41)
SHAPE_REPRESENTATION_RELATIONSHIP()
);
#189=(
REPRESENTATION_RELATIONSHIP($,$,#24170,#24166)
REPRESENTATION_RELATIONSHIP_WITH_TRANSFORMATION(#42)
SHAPE_REPRESENTATION_RELATIONSHIP()
);
#190=(
REPRESENTATION_RELATIONSHIP($,$,#24171,#24166)
REPRESENTATION_RELATIONSHIP_WITH_TRANSFORMATION(#43)
SHAPE_REPRESENTATION_RELATIONSHIP()
);
#191=(
REPRESENTATION_RELATIONSHIP($,$,#24172,#24166)
REPRESENTATION_RELATIONSHIP_WITH_TRANSFORMATION(#44)
SHAPE_REPRESENTATION_RELATIONSHIP()
);
#192=(
REPRESENTATION_RELATIONSHIP($,$,#24173,#24166)
REPRESENTATION_RELATIONSHIP_WITH_TRANSFORMATION(#45)
SHAPE_REPRESENTATION_RELATIONSHIP()
);
#193=(
REPRESENTATION_RELATIONSHIP($,$,#24174,#24166)
REPRESENTATION_RELATIONSHIP_WITH_TRANSFORMATION(#46)
SHAPE_REPRESENTATION_RELATIONSHIP()
);
#194=(
REPRESENTATION_RELATIONSHIP($,$,#24175,#24166)
REPRESENTATION_RELATIONSHIP_WITH_TRANSFORMATION(#47)
SHAPE_REPRESENTATION_RELATIONSHIP()
);
#195=(
REPRESENTATION_RELATIONSHIP($,$,#24176,#24166)
REPRESENTATION_RELATIONSHIP_WITH_TRANSFORMATION(#48)
SHAPE_REPRESENTATION_RELATIONSHIP()
);
#196=(
REPRESENTATION_RELATIONSHIP($,$,#24177,#24166)
REPRESENTATION_RELATIONSHIP_WITH_TRANSFORMATION(#49)
SHAPE_REPRESENTATION_RELATIONSHIP()
);
#197=(
REPRESENTATION_RELATIONSHIP($,$,#24178,#24166)
REPRESENTATION_RELATIONSHIP_WITH_TRANSFORMATION(#50)
SHAPE_REPRESENTATION_RELATIONSHIP()
);
#198=(
REPRESENTATION_RELATIONSHIP($,$,#24179,#24166)
REPRESENTATION_RELATIONSHIP_WITH_TRANSFORMATION(#51)
SHAPE_REPRESENTATION_RELATIONSHIP()
);
#199=(
REPRESENTATION_RELATIONSHIP($,$,#24180,#24166)
REPRESENTATION_RELATIONSHIP_WITH_TRANSFORMATION(#52)
SHAPE_REPRESENTATION_RELATIONSHIP()
);
#200=(
REPRESENTATION_RELATIONSHIP($,$,#24181,#24166)
REPRESENTATION_RELATIONSHIP_WITH_TRANSFORMATION(#53)
SHAPE_REPRESENTATION_RELATIONSHIP()
);
#201=(
REPRESENTATION_RELATIONSHIP($,$,#24182,#24166)
REPRESENTATION_RELATIONSHIP_WITH_TRANSFORMATION(#54)
SHAPE_REPRESENTATION_RELATIONSHIP()
);
#202=(
REPRESENTATION_RELATIONSHIP($,$,#24183,#24166)
REPRESENTATION_RELATIONSHIP_WITH_TRANSFORMATION(#55)
SHAPE_REPRESENTATION_RELATIONSHIP()
);
#203=(
REPRESENTATION_RELATIONSHIP($,$,#24184,#24166)
REPRESENTATION_RELATIONSHIP_WITH_TRANSFORMATION(#56)
SHAPE_REPRESENTATION_RELATIONSHIP()
);
#204=(
REPRESENTATION_RELATIONSHIP($,$,#24185,#24166)
REPRESENTATION_RELATIONSHIP_WITH_TRANSFORMATION(#57)
SHAPE_REPRESENTATION_RELATIONSHIP()
);
#205=(
REPRESENTATION_RELATIONSHIP($,$,#24186,#24166)
REPRESENTATION_RELATIONSHIP_WITH_TRANSFORMATION(#58)
SHAPE_REPRESENTATION_RELATIONSHIP()
);
#206=(
REPRESENTATION_RELATIONSHIP($,$,#24187,#24166)
REPRESENTATION_RELATIONSHIP_WITH_TRANSFORMATION(#59)
SHAPE_REPRESENTATION_RELATIONSHIP()
);
#207=(
REPRESENTATION_RELATIONSHIP($,$,#24188,#24166)
REPRESENTATION_RELATIONSHIP_WITH_TRANSFORMATION(#60)
SHAPE_REPRESENTATION_RELATIONSHIP()
);
#208=(
REPRESENTATION_RELATIONSHIP($,$,#24188,#24166)
REPRESENTATION_RELATIONSHIP_WITH_TRANSFORMATION(#61)
SHAPE_REPRESENTATION_RELATIONSHIP()
);
#209=(
REPRESENTATION_RELATIONSHIP($,$,#24114,#24113)
REPRESENTATION_RELATIONSHIP_WITH_TRANSFORMATION(#62)
SHAPE_REPRESENTATION_RELATIONSHIP()
);
#210=(
REPRESENTATION_RELATIONSHIP($,$,#24115,#24113)
REPRESENTATION_RELATIONSHIP_WITH_TRANSFORMATION(#63)
SHAPE_REPRESENTATION_RELATIONSHIP()
);
#211=(
REPRESENTATION_RELATIONSHIP($,$,#24116,#24113)
REPRESENTATION_RELATIONSHIP_WITH_TRANSFORMATION(#64)
SHAPE_REPRESENTATION_RELATIONSHIP()
);
#212=(
REPRESENTATION_RELATIONSHIP($,$,#24117,#24113)
REPRESENTATION_RELATIONSHIP_WITH_TRANSFORMATION(#65)
SHAPE_REPRESENTATION_RELATIONSHIP()
);
#213=(
REPRESENTATION_RELATIONSHIP($,$,#24118,#24113)
REPRESENTATION_RELATIONSHIP_WITH_TRANSFORMATION(#66)
SHAPE_REPRESENTATION_RELATIONSHIP()
);
#214=(
REPRESENTATION_RELATIONSHIP($,$,#24119,#24113)
REPRESENTATION_RELATIONSHIP_WITH_TRANSFORMATION(#67)
SHAPE_REPRESENTATION_RELATIONSHIP()
);
#215=(
REPRESENTATION_RELATIONSHIP($,$,#24120,#24113)
REPRESENTATION_RELATIONSHIP_WITH_TRANSFORMATION(#68)
SHAPE_REPRESENTATION_RELATIONSHIP()
);
#216=(
REPRESENTATION_RELATIONSHIP($,$,#24121,#24113)
REPRESENTATION_RELATIONSHIP_WITH_TRANSFORMATION(#69)
SHAPE_REPRESENTATION_RELATIONSHIP()
);
#217=(
REPRESENTATION_RELATIONSHIP($,$,#24122,#24113)
REPRESENTATION_RELATIONSHIP_WITH_TRANSFORMATION(#70)
SHAPE_REPRESENTATION_RELATIONSHIP()
);
#218=(
REPRESENTATION_RELATIONSHIP($,$,#24123,#24113)
REPRESENTATION_RELATIONSHIP_WITH_TRANSFORMATION(#71)
SHAPE_REPRESENTATION_RELATIONSHIP()
);
#219=(
REPRESENTATION_RELATIONSHIP($,$,#24124,#24113)
REPRESENTATION_RELATIONSHIP_WITH_TRANSFORMATION(#72)
SHAPE_REPRESENTATION_RELATIONSHIP()
);
#220=(
REPRESENTATION_RELATIONSHIP($,$,#24125,#24113)
REPRESENTATION_RELATIONSHIP_WITH_TRANSFORMATION(#73)
SHAPE_REPRESENTATION_RELATIONSHIP()
);
#221=(
REPRESENTATION_RELATIONSHIP($,$,#24126,#24113)
REPRESENTATION_RELATIONSHIP_WITH_TRANSFORMATION(#74)
SHAPE_REPRESENTATION_RELATIONSHIP()
);
#222=(
REPRESENTATION_RELATIONSHIP($,$,#24127,#24113)
REPRESENTATION_RELATIONSHIP_WITH_TRANSFORMATION(#75)
SHAPE_REPRESENTATION_RELATIONSHIP()
);
#223=(
REPRESENTATION_RELATIONSHIP($,$,#24128,#24113)
REPRESENTATION_RELATIONSHIP_WITH_TRANSFORMATION(#76)
SHAPE_REPRESENTATION_RELATIONSHIP()
);
#224=(
REPRESENTATION_RELATIONSHIP($,$,#24129,#24113)
REPRESENTATION_RELATIONSHIP_WITH_TRANSFORMATION(#77)
SHAPE_REPRESENTATION_RELATIONSHIP()
);
#225=(
REPRESENTATION_RELATIONSHIP($,$,#24130,#24113)
REPRESENTATION_RELATIONSHIP_WITH_TRANSFORMATION(#78)
SHAPE_REPRESENTATION_RELATIONSHIP()
);
#226=(
REPRESENTATION_RELATIONSHIP($,$,#24131,#24113)
REPRESENTATION_RELATIONSHIP_WITH_TRANSFORMATION(#79)
SHAPE_REPRESENTATION_RELATIONSHIP()
);
#227=(
REPRESENTATION_RELATIONSHIP($,$,#24132,#24113)
REPRESENTATION_RELATIONSHIP_WITH_TRANSFORMATION(#80)
SHAPE_REPRESENTATION_RELATIONSHIP()
);
#228=(
REPRESENTATION_RELATIONSHIP($,$,#24133,#24113)
REPRESENTATION_RELATIONSHIP_WITH_TRANSFORMATION(#81)
SHAPE_REPRESENTATION_RELATIONSHIP()
);
#229=(
REPRESENTATION_RELATIONSHIP($,$,#24134,#24113)
REPRESENTATION_RELATIONSHIP_WITH_TRANSFORMATION(#82)
SHAPE_REPRESENTATION_RELATIONSHIP()
);
#230=(
REPRESENTATION_RELATIONSHIP($,$,#24135,#24113)
REPRESENTATION_RELATIONSHIP_WITH_TRANSFORMATION(#83)
SHAPE_REPRESENTATION_RELATIONSHIP()
);
#231=(
REPRESENTATION_RELATIONSHIP($,$,#24136,#24113)
REPRESENTATION_RELATIONSHIP_WITH_TRANSFORMATION(#84)
SHAPE_REPRESENTATION_RELATIONSHIP()
);
#232=(
REPRESENTATION_RELATIONSHIP($,$,#24137,#24113)
REPRESENTATION_RELATIONSHIP_WITH_TRANSFORMATION(#85)
SHAPE_REPRESENTATION_RELATIONSHIP()
);
#233=(
REPRESENTATION_RELATIONSHIP($,$,#24138,#24113)
REPRESENTATION_RELATIONSHIP_WITH_TRANSFORMATION(#86)
SHAPE_REPRESENTATION_RELATIONSHIP()
);
#234=(
REPRESENTATION_RELATIONSHIP($,$,#24139,#24113)
REPRESENTATION_RELATIONSHIP_WITH_TRANSFORMATION(#87)
SHAPE_REPRESENTATION_RELATIONSHIP()
);
#235=(
REPRESENTATION_RELATIONSHIP($,$,#24140,#24113)
REPRESENTATION_RELATIONSHIP_WITH_TRANSFORMATION(#88)
SHAPE_REPRESENTATION_RELATIONSHIP()
);
#236=(
REPRESENTATION_RELATIONSHIP($,$,#24141,#24113)
REPRESENTATION_RELATIONSHIP_WITH_TRANSFORMATION(#89)
SHAPE_REPRESENTATION_RELATIONSHIP()
);
#237=(
REPRESENTATION_RELATIONSHIP($,$,#24142,#24113)
REPRESENTATION_RELATIONSHIP_WITH_TRANSFORMATION(#90)
SHAPE_REPRESENTATION_RELATIONSHIP()
);
#238=(
REPRESENTATION_RELATIONSHIP($,$,#24143,#24113)
REPRESENTATION_RELATIONSHIP_WITH_TRANSFORMATION(#91)
SHAPE_REPRESENTATION_RELATIONSHIP()
);
#239=(
REPRESENTATION_RELATIONSHIP($,$,#24143,#24113)
REPRESENTATION_RELATIONSHIP_WITH_TRANSFORMATION(#92)
SHAPE_REPRESENTATION_RELATIONSHIP()
);
#240=(
REPRESENTATION_RELATIONSHIP($,$,#24143,#24113)
REPRESENTATION_RELATIONSHIP_WITH_TRANSFORMATION(#93)
SHAPE_REPRESENTATION_RELATIONSHIP()
);
#241=(
REPRESENTATION_RELATIONSHIP($,$,#24143,#24113)
REPRESENTATION_RELATIONSHIP_WITH_TRANSFORMATION(#94)
SHAPE_REPRESENTATION_RELATIONSHIP()
);
#242=(
REPRESENTATION_RELATIONSHIP($,$,#24143,#24113)
REPRESENTATION_RELATIONSHIP_WITH_TRANSFORMATION(#95)
SHAPE_REPRESENTATION_RELATIONSHIP()
);
#243=(
REPRESENTATION_RELATIONSHIP($,$,#24143,#24113)
REPRESENTATION_RELATIONSHIP_WITH_TRANSFORMATION(#96)
SHAPE_REPRESENTATION_RELATIONSHIP()
);
#244=(
REPRESENTATION_RELATIONSHIP($,$,#24143,#24113)
REPRESENTATION_RELATIONSHIP_WITH_TRANSFORMATION(#97)
SHAPE_REPRESENTATION_RELATIONSHIP()
);
#245=(
REPRESENTATION_RELATIONSHIP($,$,#24143,#24113)
REPRESENTATION_RELATIONSHIP_WITH_TRANSFORMATION(#98)
SHAPE_REPRESENTATION_RELATIONSHIP()
);
#246=(
REPRESENTATION_RELATIONSHIP($,$,#24207,#24113)
REPRESENTATION_RELATIONSHIP_WITH_TRANSFORMATION(#99)
SHAPE_REPRESENTATION_RELATIONSHIP()
);
#247=(
REPRESENTATION_RELATIONSHIP($,$,#24207,#24113)
REPRESENTATION_RELATIONSHIP_WITH_TRANSFORMATION(#100)
SHAPE_REPRESENTATION_RELATIONSHIP()
);
#248=(
REPRESENTATION_RELATIONSHIP($,$,#24207,#24113)
REPRESENTATION_RELATIONSHIP_WITH_TRANSFORMATION(#101)
SHAPE_REPRESENTATION_RELATIONSHIP()
);
#249=(
REPRESENTATION_RELATIONSHIP($,$,#24207,#24113)
REPRESENTATION_RELATIONSHIP_WITH_TRANSFORMATION(#102)
SHAPE_REPRESENTATION_RELATIONSHIP()
);
#250=(
REPRESENTATION_RELATIONSHIP($,$,#24207,#24113)
REPRESENTATION_RELATIONSHIP_WITH_TRANSFORMATION(#103)
SHAPE_REPRESENTATION_RELATIONSHIP()
);
#251=(
REPRESENTATION_RELATIONSHIP($,$,#24207,#24113)
REPRESENTATION_RELATIONSHIP_WITH_TRANSFORMATION(#104)
SHAPE_REPRESENTATION_RELATIONSHIP()
);
#252=(
REPRESENTATION_RELATIONSHIP($,$,#24207,#24113)
REPRESENTATION_RELATIONSHIP_WITH_TRANSFORMATION(#105)
SHAPE_REPRESENTATION_RELATIONSHIP()
);
#253=(
REPRESENTATION_RELATIONSHIP($,$,#24207,#24113)
REPRESENTATION_RELATIONSHIP_WITH_TRANSFORMATION(#106)
SHAPE_REPRESENTATION_RELATIONSHIP()
);
#254=(
REPRESENTATION_RELATIONSHIP($,$,#24188,#24113)
REPRESENTATION_RELATIONSHIP_WITH_TRANSFORMATION(#107)
SHAPE_REPRESENTATION_RELATIONSHIP()
);
#255=(
REPRESENTATION_RELATIONSHIP($,$,#24207,#24113)
REPRESENTATION_RELATIONSHIP_WITH_TRANSFORMATION(#108)
SHAPE_REPRESENTATION_RELATIONSHIP()
);
#256=(
REPRESENTATION_RELATIONSHIP($,$,#24207,#24113)
REPRESENTATION_RELATIONSHIP_WITH_TRANSFORMATION(#109)
SHAPE_REPRESENTATION_RELATIONSHIP()
);
#257=(
REPRESENTATION_RELATIONSHIP($,$,#24188,#24113)
REPRESENTATION_RELATIONSHIP_WITH_TRANSFORMATION(#110)
SHAPE_REPRESENTATION_RELATIONSHIP()
);
#258=(
REPRESENTATION_RELATIONSHIP($,$,#24207,#24113)
REPRESENTATION_RELATIONSHIP_WITH_TRANSFORMATION(#111)
SHAPE_REPRESENTATION_RELATIONSHIP()
);
#259=(
REPRESENTATION_RELATIONSHIP($,$,#24207,#24113)
REPRESENTATION_RELATIONSHIP_WITH_TRANSFORMATION(#112)
SHAPE_REPRESENTATION_RELATIONSHIP()
);
#260=(
REPRESENTATION_RELATIONSHIP($,$,#24195,#24194)
REPRESENTATION_RELATIONSHIP_WITH_TRANSFORMATION(#113)
SHAPE_REPRESENTATION_RELATIONSHIP()
);
#261=(
REPRESENTATION_RELATIONSHIP($,$,#24196,#24194)
REPRESENTATION_RELATIONSHIP_WITH_TRANSFORMATION(#114)
SHAPE_REPRESENTATION_RELATIONSHIP()
);
#262=(
REPRESENTATION_RELATIONSHIP($,$,#24197,#24194)
REPRESENTATION_RELATIONSHIP_WITH_TRANSFORMATION(#115)
SHAPE_REPRESENTATION_RELATIONSHIP()
);
#263=(
REPRESENTATION_RELATIONSHIP($,$,#24198,#24194)
REPRESENTATION_RELATIONSHIP_WITH_TRANSFORMATION(#116)
SHAPE_REPRESENTATION_RELATIONSHIP()
);
#264=(
REPRESENTATION_RELATIONSHIP($,$,#24199,#24194)
REPRESENTATION_RELATIONSHIP_WITH_TRANSFORMATION(#117)
SHAPE_REPRESENTATION_RELATIONSHIP()
);
#265=(
REPRESENTATION_RELATIONSHIP($,$,#24200,#24194)
REPRESENTATION_RELATIONSHIP_WITH_TRANSFORMATION(#118)
SHAPE_REPRESENTATION_RELATIONSHIP()
);
#266=(
REPRESENTATION_RELATIONSHIP($,$,#24201,#24194)
REPRESENTATION_RELATIONSHIP_WITH_TRANSFORMATION(#119)
SHAPE_REPRESENTATION_RELATIONSHIP()
);
#267=(
REPRESENTATION_RELATIONSHIP($,$,#24202,#24194)
REPRESENTATION_RELATIONSHIP_WITH_TRANSFORMATION(#120)
SHAPE_REPRESENTATION_RELATIONSHIP()
);
#268=(
REPRESENTATION_RELATIONSHIP($,$,#24203,#24194)
REPRESENTATION_RELATIONSHIP_WITH_TRANSFORMATION(#121)
SHAPE_REPRESENTATION_RELATIONSHIP()
);
#269=(
REPRESENTATION_RELATIONSHIP($,$,#24204,#24194)
REPRESENTATION_RELATIONSHIP_WITH_TRANSFORMATION(#122)
SHAPE_REPRESENTATION_RELATIONSHIP()
);
#270=(
REPRESENTATION_RELATIONSHIP($,$,#24205,#24194)
REPRESENTATION_RELATIONSHIP_WITH_TRANSFORMATION(#123)
SHAPE_REPRESENTATION_RELATIONSHIP()
);
#271=(
REPRESENTATION_RELATIONSHIP($,$,#24206,#24194)
REPRESENTATION_RELATIONSHIP_WITH_TRANSFORMATION(#124)
SHAPE_REPRESENTATION_RELATIONSHIP()
);
#272=(
REPRESENTATION_RELATIONSHIP($,$,#24207,#24194)
REPRESENTATION_RELATIONSHIP_WITH_TRANSFORMATION(#125)
SHAPE_REPRESENTATION_RELATIONSHIP()
);
#273=(
REPRESENTATION_RELATIONSHIP($,$,#24207,#24194)
REPRESENTATION_RELATIONSHIP_WITH_TRANSFORMATION(#126)
SHAPE_REPRESENTATION_RELATIONSHIP()
);
#274=(
REPRESENTATION_RELATIONSHIP($,$,#24207,#24194)
REPRESENTATION_RELATIONSHIP_WITH_TRANSFORMATION(#127)
SHAPE_REPRESENTATION_RELATIONSHIP()
);
#275=(
REPRESENTATION_RELATIONSHIP($,$,#24207,#24194)
REPRESENTATION_RELATIONSHIP_WITH_TRANSFORMATION(#128)
SHAPE_REPRESENTATION_RELATIONSHIP()
);
#276=(
REPRESENTATION_RELATIONSHIP($,$,#24207,#24194)
REPRESENTATION_RELATIONSHIP_WITH_TRANSFORMATION(#129)
SHAPE_REPRESENTATION_RELATIONSHIP()
);
#277=(
REPRESENTATION_RELATIONSHIP($,$,#24207,#24194)
REPRESENTATION_RELATIONSHIP_WITH_TRANSFORMATION(#130)
SHAPE_REPRESENTATION_RELATIONSHIP()
);
#278=(
REPRESENTATION_RELATIONSHIP($,$,#24207,#24194)
REPRESENTATION_RELATIONSHIP_WITH_TRANSFORMATION(#131)
SHAPE_REPRESENTATION_RELATIONSHIP()
);
#279=(
REPRESENTATION_RELATIONSHIP($,$,#24207,#24194)
REPRESENTATION_RELATIONSHIP_WITH_TRANSFORMATION(#132)
SHAPE_REPRESENTATION_RELATIONSHIP()
);
#280=(
REPRESENTATION_RELATIONSHIP($,$,#24217,#24216)
REPRESENTATION_RELATIONSHIP_WITH_TRANSFORMATION(#133)
SHAPE_REPRESENTATION_RELATIONSHIP()
);
#281=(
REPRESENTATION_RELATIONSHIP($,$,#24218,#24216)
REPRESENTATION_RELATIONSHIP_WITH_TRANSFORMATION(#134)
SHAPE_REPRESENTATION_RELATIONSHIP()
);
#282=(
REPRESENTATION_RELATIONSHIP($,$,#24209,#24208)
REPRESENTATION_RELATIONSHIP_WITH_TRANSFORMATION(#135)
SHAPE_REPRESENTATION_RELATIONSHIP()
);
#283=(
REPRESENTATION_RELATIONSHIP($,$,#24210,#24208)
REPRESENTATION_RELATIONSHIP_WITH_TRANSFORMATION(#136)
SHAPE_REPRESENTATION_RELATIONSHIP()
);
#284=(
REPRESENTATION_RELATIONSHIP($,$,#24211,#24208)
REPRESENTATION_RELATIONSHIP_WITH_TRANSFORMATION(#137)
SHAPE_REPRESENTATION_RELATIONSHIP()
);
#285=(
REPRESENTATION_RELATIONSHIP($,$,#24212,#24208)
REPRESENTATION_RELATIONSHIP_WITH_TRANSFORMATION(#138)
SHAPE_REPRESENTATION_RELATIONSHIP()
);
#286=(
REPRESENTATION_RELATIONSHIP($,$,#24213,#24208)
REPRESENTATION_RELATIONSHIP_WITH_TRANSFORMATION(#139)
SHAPE_REPRESENTATION_RELATIONSHIP()
);
#287=(
REPRESENTATION_RELATIONSHIP($,$,#24214,#24208)
REPRESENTATION_RELATIONSHIP_WITH_TRANSFORMATION(#140)
SHAPE_REPRESENTATION_RELATIONSHIP()
);
#288=(
REPRESENTATION_RELATIONSHIP($,$,#24215,#24208)
REPRESENTATION_RELATIONSHIP_WITH_TRANSFORMATION(#141)
SHAPE_REPRESENTATION_RELATIONSHIP()
);
#289=(
REPRESENTATION_RELATIONSHIP($,$,#24216,#24208)
REPRESENTATION_RELATIONSHIP_WITH_TRANSFORMATION(#142)
SHAPE_REPRESENTATION_RELATIONSHIP()
);
#290=(
REPRESENTATION_RELATIONSHIP($,$,#24216,#24208)
REPRESENTATION_RELATIONSHIP_WITH_TRANSFORMATION(#143)
SHAPE_REPRESENTATION_RELATIONSHIP()
);
#291=(
REPRESENTATION_RELATIONSHIP($,$,#24219,#24208)
REPRESENTATION_RELATIONSHIP_WITH_TRANSFORMATION(#144)
SHAPE_REPRESENTATION_RELATIONSHIP()
);
#292=(
REPRESENTATION_RELATIONSHIP($,$,#24221,#24220)
REPRESENTATION_RELATIONSHIP_WITH_TRANSFORMATION(#145)
SHAPE_REPRESENTATION_RELATIONSHIP()
);
#293=(
REPRESENTATION_RELATIONSHIP($,$,#24223,#24222)
REPRESENTATION_RELATIONSHIP_WITH_TRANSFORMATION(#146)
SHAPE_REPRESENTATION_RELATIONSHIP()
);
#294=(
REPRESENTATION_RELATIONSHIP($,$,#24224,#24222)
REPRESENTATION_RELATIONSHIP_WITH_TRANSFORMATION(#147)
SHAPE_REPRESENTATION_RELATIONSHIP()
);
#295=(
REPRESENTATION_RELATIONSHIP($,$,#24225,#24222)
REPRESENTATION_RELATIONSHIP_WITH_TRANSFORMATION(#148)
SHAPE_REPRESENTATION_RELATIONSHIP()
);
#296=(
REPRESENTATION_RELATIONSHIP($,$,#24226,#24222)
REPRESENTATION_RELATIONSHIP_WITH_TRANSFORMATION(#149)
SHAPE_REPRESENTATION_RELATIONSHIP()
);
#297=(
REPRESENTATION_RELATIONSHIP($,$,#24227,#24222)
REPRESENTATION_RELATIONSHIP_WITH_TRANSFORMATION(#150)
SHAPE_REPRESENTATION_RELATIONSHIP()
);
#298=(
REPRESENTATION_RELATIONSHIP($,$,#24113,#24112)
REPRESENTATION_RELATIONSHIP_WITH_TRANSFORMATION(#151)
SHAPE_REPRESENTATION_RELATIONSHIP()
);
#299=(
REPRESENTATION_RELATIONSHIP($,$,#24144,#24112)
REPRESENTATION_RELATIONSHIP_WITH_TRANSFORMATION(#152)
SHAPE_REPRESENTATION_RELATIONSHIP()
);
#300=(
REPRESENTATION_RELATIONSHIP($,$,#24166,#24112)
REPRESENTATION_RELATIONSHIP_WITH_TRANSFORMATION(#153)
SHAPE_REPRESENTATION_RELATIONSHIP()
);
#301=(
REPRESENTATION_RELATIONSHIP($,$,#24194,#24112)
REPRESENTATION_RELATIONSHIP_WITH_TRANSFORMATION(#154)
SHAPE_REPRESENTATION_RELATIONSHIP()
);
#302=(
REPRESENTATION_RELATIONSHIP($,$,#24208,#24112)
REPRESENTATION_RELATIONSHIP_WITH_TRANSFORMATION(#155)
SHAPE_REPRESENTATION_RELATIONSHIP()
);
#303=(
REPRESENTATION_RELATIONSHIP($,$,#24220,#24112)
REPRESENTATION_RELATIONSHIP_WITH_TRANSFORMATION(#156)
SHAPE_REPRESENTATION_RELATIONSHIP()
);
#304=(
REPRESENTATION_RELATIONSHIP($,$,#24222,#24112)
REPRESENTATION_RELATIONSHIP_WITH_TRANSFORMATION(#157)
SHAPE_REPRESENTATION_RELATIONSHIP()
);
#305=CONTEXT_DEPENDENT_SHAPE_REPRESENTATION(#158,#23931);
#306=CONTEXT_DEPENDENT_SHAPE_REPRESENTATION(#159,#23932);
#307=CONTEXT_DEPENDENT_SHAPE_REPRESENTATION(#160,#23933);
#308=CONTEXT_DEPENDENT_SHAPE_REPRESENTATION(#161,#23934);
#309=CONTEXT_DEPENDENT_SHAPE_REPRESENTATION(#162,#23935);
#310=CONTEXT_DEPENDENT_SHAPE_REPRESENTATION(#163,#23936);
#311=CONTEXT_DEPENDENT_SHAPE_REPRESENTATION(#164,#23937);
#312=CONTEXT_DEPENDENT_SHAPE_REPRESENTATION(#165,#23938);
#313=CONTEXT_DEPENDENT_SHAPE_REPRESENTATION(#166,#23939);
#314=CONTEXT_DEPENDENT_SHAPE_REPRESENTATION(#167,#23940);
#315=CONTEXT_DEPENDENT_SHAPE_REPRESENTATION(#168,#23941);
#316=CONTEXT_DEPENDENT_SHAPE_REPRESENTATION(#169,#23942);
#317=CONTEXT_DEPENDENT_SHAPE_REPRESENTATION(#170,#23943);
#318=CONTEXT_DEPENDENT_SHAPE_REPRESENTATION(#171,#23944);
#319=CONTEXT_DEPENDENT_SHAPE_REPRESENTATION(#172,#23945);
#320=CONTEXT_DEPENDENT_SHAPE_REPRESENTATION(#173,#23946);
#321=CONTEXT_DEPENDENT_SHAPE_REPRESENTATION(#174,#23947);
#322=CONTEXT_DEPENDENT_SHAPE_REPRESENTATION(#175,#23948);
#323=CONTEXT_DEPENDENT_SHAPE_REPRESENTATION(#176,#23949);
#324=CONTEXT_DEPENDENT_SHAPE_REPRESENTATION(#177,#23950);
#325=CONTEXT_DEPENDENT_SHAPE_REPRESENTATION(#178,#23951);
#326=CONTEXT_DEPENDENT_SHAPE_REPRESENTATION(#179,#23952);
#327=CONTEXT_DEPENDENT_SHAPE_REPRESENTATION(#180,#23953);
#328=CONTEXT_DEPENDENT_SHAPE_REPRESENTATION(#181,#23954);
#329=CONTEXT_DEPENDENT_SHAPE_REPRESENTATION(#182,#23955);
#330=CONTEXT_DEPENDENT_SHAPE_REPRESENTATION(#183,#23956);
#331=CONTEXT_DEPENDENT_SHAPE_REPRESENTATION(#184,#23957);
#332=CONTEXT_DEPENDENT_SHAPE_REPRESENTATION(#185,#23958);
#333=CONTEXT_DEPENDENT_SHAPE_REPRESENTATION(#186,#23959);
#334=CONTEXT_DEPENDENT_SHAPE_REPRESENTATION(#187,#23960);
#335=CONTEXT_DEPENDENT_SHAPE_REPRESENTATION(#188,#23961);
#336=CONTEXT_DEPENDENT_SHAPE_REPRESENTATION(#189,#23962);
#337=CONTEXT_DEPENDENT_SHAPE_REPRESENTATION(#190,#23963);
#338=CONTEXT_DEPENDENT_SHAPE_REPRESENTATION(#191,#23964);
#339=CONTEXT_DEPENDENT_SHAPE_REPRESENTATION(#192,#23965);
#340=CONTEXT_DEPENDENT_SHAPE_REPRESENTATION(#193,#23966);
#341=CONTEXT_DEPENDENT_SHAPE_REPRESENTATION(#194,#23967);
#342=CONTEXT_DEPENDENT_SHAPE_REPRESENTATION(#195,#23968);
#343=CONTEXT_DEPENDENT_SHAPE_REPRESENTATION(#196,#23969);
#344=CONTEXT_DEPENDENT_SHAPE_REPRESENTATION(#197,#23970);
#345=CONTEXT_DEPENDENT_SHAPE_REPRESENTATION(#198,#23971);
#346=CONTEXT_DEPENDENT_SHAPE_REPRESENTATION(#199,#23972);
#347=CONTEXT_DEPENDENT_SHAPE_REPRESENTATION(#200,#23973);
#348=CONTEXT_DEPENDENT_SHAPE_REPRESENTATION(#201,#23974);
#349=CONTEXT_DEPENDENT_SHAPE_REPRESENTATION(#202,#23975);
#350=CONTEXT_DEPENDENT_SHAPE_REPRESENTATION(#203,#23976);
#351=CONTEXT_DEPENDENT_SHAPE_REPRESENTATION(#204,#23977);
#352=CONTEXT_DEPENDENT_SHAPE_REPRESENTATION(#205,#23978);
#353=CONTEXT_DEPENDENT_SHAPE_REPRESENTATION(#206,#23979);
#354=CONTEXT_DEPENDENT_SHAPE_REPRESENTATION(#207,#23980);
#355=CONTEXT_DEPENDENT_SHAPE_REPRESENTATION(#208,#23981);
#356=CONTEXT_DEPENDENT_SHAPE_REPRESENTATION(#209,#23996);
#357=CONTEXT_DEPENDENT_SHAPE_REPRESENTATION(#210,#23997);
#358=CONTEXT_DEPENDENT_SHAPE_REPRESENTATION(#211,#23998);
#359=CONTEXT_DEPENDENT_SHAPE_REPRESENTATION(#212,#23999);
#360=CONTEXT_DEPENDENT_SHAPE_REPRESENTATION(#213,#24000);
#361=CONTEXT_DEPENDENT_SHAPE_REPRESENTATION(#214,#24001);
#362=CONTEXT_DEPENDENT_SHAPE_REPRESENTATION(#215,#24002);
#363=CONTEXT_DEPENDENT_SHAPE_REPRESENTATION(#216,#24003);
#364=CONTEXT_DEPENDENT_SHAPE_REPRESENTATION(#217,#24004);
#365=CONTEXT_DEPENDENT_SHAPE_REPRESENTATION(#218,#24005);
#366=CONTEXT_DEPENDENT_SHAPE_REPRESENTATION(#219,#24006);
#367=CONTEXT_DEPENDENT_SHAPE_REPRESENTATION(#220,#24007);
#368=CONTEXT_DEPENDENT_SHAPE_REPRESENTATION(#221,#24008);
#369=CONTEXT_DEPENDENT_SHAPE_REPRESENTATION(#222,#24009);
#370=CONTEXT_DEPENDENT_SHAPE_REPRESENTATION(#223,#24010);
#371=CONTEXT_DEPENDENT_SHAPE_REPRESENTATION(#224,#24011);
#372=CONTEXT_DEPENDENT_SHAPE_REPRESENTATION(#225,#24012);
#373=CONTEXT_DEPENDENT_SHAPE_REPRESENTATION(#226,#24013);
#374=CONTEXT_DEPENDENT_SHAPE_REPRESENTATION(#227,#24014);
#375=CONTEXT_DEPENDENT_SHAPE_REPRESENTATION(#228,#24015);
#376=CONTEXT_DEPENDENT_SHAPE_REPRESENTATION(#229,#24016);
#377=CONTEXT_DEPENDENT_SHAPE_REPRESENTATION(#230,#24017);
#378=CONTEXT_DEPENDENT_SHAPE_REPRESENTATION(#231,#24018);
#379=CONTEXT_DEPENDENT_SHAPE_REPRESENTATION(#232,#24019);
#380=CONTEXT_DEPENDENT_SHAPE_REPRESENTATION(#233,#24020);
#381=CONTEXT_DEPENDENT_SHAPE_REPRESENTATION(#234,#24021);
#382=CONTEXT_DEPENDENT_SHAPE_REPRESENTATION(#235,#24022);
#383=CONTEXT_DEPENDENT_SHAPE_REPRESENTATION(#236,#24023);
#384=CONTEXT_DEPENDENT_SHAPE_REPRESENTATION(#237,#24024);
#385=CONTEXT_DEPENDENT_SHAPE_REPRESENTATION(#238,#24025);
#386=CONTEXT_DEPENDENT_SHAPE_REPRESENTATION(#239,#24026);
#387=CONTEXT_DEPENDENT_SHAPE_REPRESENTATION(#240,#24027);
#388=CONTEXT_DEPENDENT_SHAPE_REPRESENTATION(#241,#24028);
#389=CONTEXT_DEPENDENT_SHAPE_REPRESENTATION(#242,#24029);
#390=CONTEXT_DEPENDENT_SHAPE_REPRESENTATION(#243,#24030);
#391=CONTEXT_DEPENDENT_SHAPE_REPRESENTATION(#244,#24031);
#392=CONTEXT_DEPENDENT_SHAPE_REPRESENTATION(#245,#24032);
#393=CONTEXT_DEPENDENT_SHAPE_REPRESENTATION(#246,#24033);
#394=CONTEXT_DEPENDENT_SHAPE_REPRESENTATION(#247,#24034);
#395=CONTEXT_DEPENDENT_SHAPE_REPRESENTATION(#248,#24035);
#396=CONTEXT_DEPENDENT_SHAPE_REPRESENTATION(#249,#24036);
#397=CONTEXT_DEPENDENT_SHAPE_REPRESENTATION(#250,#24037);
#398=CONTEXT_DEPENDENT_SHAPE_REPRESENTATION(#251,#24038);
#399=CONTEXT_DEPENDENT_SHAPE_REPRESENTATION(#252,#24039);
#400=CONTEXT_DEPENDENT_SHAPE_REPRESENTATION(#253,#24040);
#401=CONTEXT_DEPENDENT_SHAPE_REPRESENTATION(#254,#24041);
#402=CONTEXT_DEPENDENT_SHAPE_REPRESENTATION(#255,#24042);
#403=CONTEXT_DEPENDENT_SHAPE_REPRESENTATION(#256,#24043);
#404=CONTEXT_DEPENDENT_SHAPE_REPRESENTATION(#257,#24044);
#405=CONTEXT_DEPENDENT_SHAPE_REPRESENTATION(#258,#24045);
#406=CONTEXT_DEPENDENT_SHAPE_REPRESENTATION(#259,#24046);
#407=CONTEXT_DEPENDENT_SHAPE_REPRESENTATION(#260,#24047);
#408=CONTEXT_DEPENDENT_SHAPE_REPRESENTATION(#261,#24048);
#409=CONTEXT_DEPENDENT_SHAPE_REPRESENTATION(#262,#24049);
#410=CONTEXT_DEPENDENT_SHAPE_REPRESENTATION(#263,#24050);
#411=CONTEXT_DEPENDENT_SHAPE_REPRESENTATION(#264,#24051);
#412=CONTEXT_DEPENDENT_SHAPE_REPRESENTATION(#265,#24052);
#413=CONTEXT_DEPENDENT_SHAPE_REPRESENTATION(#266,#24053);
#414=CONTEXT_DEPENDENT_SHAPE_REPRESENTATION(#267,#24054);
#415=CONTEXT_DEPENDENT_SHAPE_REPRESENTATION(#268,#24055);
#416=CONTEXT_DEPENDENT_SHAPE_REPRESENTATION(#269,#24056);
#417=CONTEXT_DEPENDENT_SHAPE_REPRESENTATION(#270,#24057);
#418=CONTEXT_DEPENDENT_SHAPE_REPRESENTATION(#271,#24058);
#419=CONTEXT_DEPENDENT_SHAPE_REPRESENTATION(#272,#24059);
#420=CONTEXT_DEPENDENT_SHAPE_REPRESENTATION(#273,#24060);
#421=CONTEXT_DEPENDENT_SHAPE_REPRESENTATION(#274,#24061);
#422=CONTEXT_DEPENDENT_SHAPE_REPRESENTATION(#275,#24062);
#423=CONTEXT_DEPENDENT_SHAPE_REPRESENTATION(#276,#24063);
#424=CONTEXT_DEPENDENT_SHAPE_REPRESENTATION(#277,#24064);
#425=CONTEXT_DEPENDENT_SHAPE_REPRESENTATION(#278,#24065);
#426=CONTEXT_DEPENDENT_SHAPE_REPRESENTATION(#279,#24066);
#427=CONTEXT_DEPENDENT_SHAPE_REPRESENTATION(#280,#24078);
#428=CONTEXT_DEPENDENT_SHAPE_REPRESENTATION(#281,#24079);
#429=CONTEXT_DEPENDENT_SHAPE_REPRESENTATION(#282,#24081);
#430=CONTEXT_DEPENDENT_SHAPE_REPRESENTATION(#283,#24082);
#431=CONTEXT_DEPENDENT_SHAPE_REPRESENTATION(#284,#24083);
#432=CONTEXT_DEPENDENT_SHAPE_REPRESENTATION(#285,#24084);
#433=CONTEXT_DEPENDENT_SHAPE_REPRESENTATION(#286,#24085);
#434=CONTEXT_DEPENDENT_SHAPE_REPRESENTATION(#287,#24086);
#435=CONTEXT_DEPENDENT_SHAPE_REPRESENTATION(#288,#24087);
#436=CONTEXT_DEPENDENT_SHAPE_REPRESENTATION(#289,#24088);
#437=CONTEXT_DEPENDENT_SHAPE_REPRESENTATION(#290,#24089);
#438=CONTEXT_DEPENDENT_SHAPE_REPRESENTATION(#291,#24090);
#439=CONTEXT_DEPENDENT_SHAPE_REPRESENTATION(#292,#24093);
#440=CONTEXT_DEPENDENT_SHAPE_REPRESENTATION(#293,#24100);
#441=CONTEXT_DEPENDENT_SHAPE_REPRESENTATION(#294,#24101);
#442=CONTEXT_DEPENDENT_SHAPE_REPRESENTATION(#295,#24102);
#443=CONTEXT_DEPENDENT_SHAPE_REPRESENTATION(#296,#24103);
#444=CONTEXT_DEPENDENT_SHAPE_REPRESENTATION(#297,#24104);
#445=CONTEXT_DEPENDENT_SHAPE_REPRESENTATION(#298,#24105);
#446=CONTEXT_DEPENDENT_SHAPE_REPRESENTATION(#299,#24106);
#447=CONTEXT_DEPENDENT_SHAPE_REPRESENTATION(#300,#24107);
#448=CONTEXT_DEPENDENT_SHAPE_REPRESENTATION(#301,#24108);
#449=CONTEXT_DEPENDENT_SHAPE_REPRESENTATION(#302,#24109);
#450=CONTEXT_DEPENDENT_SHAPE_REPRESENTATION(#303,#24110);
#451=CONTEXT_DEPENDENT_SHAPE_REPRESENTATION(#304,#24111);
#452=NEXT_ASSEMBLY_USAGE_OCCURRENCE('Inner ring:1','Inner ring:1',
'Inner ring:1',#24305,#24306,'Inner ring:1');
#453=NEXT_ASSEMBLY_USAGE_OCCURRENCE('Outer ring:1','Outer ring:1',
'Outer ring:1',#24305,#24307,'Outer ring:1');
#454=NEXT_ASSEMBLY_USAGE_OCCURRENCE('Balls:1','Balls:1','Balls:1',#24305,
#24308,'Balls:1');
#455=NEXT_ASSEMBLY_USAGE_OCCURRENCE('Cage:1','Cage:1','Cage:1',#24305,#24309,
'Cage:1');
#456=NEXT_ASSEMBLY_USAGE_OCCURRENCE('Seals 2RS:1','Seals 2RS:1',
'Seals 2RS:1',#24305,#24310,'Seals 2RS:1');
#457=NEXT_ASSEMBLY_USAGE_OCCURRENCE('Input link (1):1',
'Input link (1):1','Input link (1):1',#24261,#24262,'Input link (1):1');
#458=NEXT_ASSEMBLY_USAGE_OCCURRENCE('Bearing cap:1','Bearing cap:1',
'Bearing cap:1',#24261,#24263,'Bearing cap:1');
#459=NEXT_ASSEMBLY_USAGE_OCCURRENCE('M4 short cap screw:1',
'M4 short cap screw:1','M4 short cap screw:1',#24261,#24264,
'M4 short cap screw:1');
#460=NEXT_ASSEMBLY_USAGE_OCCURRENCE('M4 short cap screw (1):1',
'M4 short cap screw (1):1','M4 short cap screw (1):1',#24261,#24265,
'M4 short cap screw (1):1');
#461=NEXT_ASSEMBLY_USAGE_OCCURRENCE('M4 short cap screw (2):1',
'M4 short cap screw (2):1','M4 short cap screw (2):1',#24261,#24266,
'M4 short cap screw (2):1');
#462=NEXT_ASSEMBLY_USAGE_OCCURRENCE('M4 short cap screw (3):1',
'M4 short cap screw (3):1','M4 short cap screw (3):1',#24261,#24267,
'M4 short cap screw (3):1');
#463=NEXT_ASSEMBLY_USAGE_OCCURRENCE('Bearing cap (1):1',
'Bearing cap (1):1','Bearing cap (1):1',#24261,#24268,
'Bearing cap (1):1');
#464=NEXT_ASSEMBLY_USAGE_OCCURRENCE('M4 short cap screw (4):1',
'M4 short cap screw (4):1','M4 short cap screw (4):1',#24261,#24269,
'M4 short cap screw (4):1');
#465=NEXT_ASSEMBLY_USAGE_OCCURRENCE('M4 short cap screw (5):1',
'M4 short cap screw (5):1','M4 short cap screw (5):1',#24261,#24270,
'M4 short cap screw (5):1');
#466=NEXT_ASSEMBLY_USAGE_OCCURRENCE('M4 short cap screw (6):1',
'M4 short cap screw (6):1','M4 short cap screw (6):1',#24261,#24271,
'M4 short cap screw (6):1');
#467=NEXT_ASSEMBLY_USAGE_OCCURRENCE('M4 short cap screw (7):1',
'M4 short cap screw (7):1','M4 short cap screw (7):1',#24261,#24272,
'M4 short cap screw (7):1');
#468=NEXT_ASSEMBLY_USAGE_OCCURRENCE('Bearing cap (2):1',
'Bearing cap (2):1','Bearing cap (2):1',#24261,#24273,
'Bearing cap (2):1');
#469=NEXT_ASSEMBLY_USAGE_OCCURRENCE('M4 short cap screw (8):1',
'M4 short cap screw (8):1','M4 short cap screw (8):1',#24261,#24274,
'M4 short cap screw (8):1');
#470=NEXT_ASSEMBLY_USAGE_OCCURRENCE('M4 short cap screw (9):1',
'M4 short cap screw (9):1','M4 short cap screw (9):1',#24261,#24275,
'M4 short cap screw (9):1');
#471=NEXT_ASSEMBLY_USAGE_OCCURRENCE('M4 short cap screw (10):1',
'M4 short cap screw (10):1','M4 short cap screw (10):1',#24261,#24276,
'M4 short cap screw (10):1');
#472=NEXT_ASSEMBLY_USAGE_OCCURRENCE('M4 short cap screw (11):1',
'M4 short cap screw (11):1','M4 short cap screw (11):1',#24261,#24277,
'M4 short cap screw (11):1');
#473=NEXT_ASSEMBLY_USAGE_OCCURRENCE('Bearing cap (3):1',
'Bearing cap (3):1','Bearing cap (3):1',#24261,#24278,
'Bearing cap (3):1');
#474=NEXT_ASSEMBLY_USAGE_OCCURRENCE('M4 short cap screw (12):1',
'M4 short cap screw (12):1','M4 short cap screw (12):1',#24261,#24279,
'M4 short cap screw (12):1');
#475=NEXT_ASSEMBLY_USAGE_OCCURRENCE('M4 short cap screw (13):1',
'M4 short cap screw (13):1','M4 short cap screw (13):1',#24261,#24280,
'M4 short cap screw (13):1');
#476=NEXT_ASSEMBLY_USAGE_OCCURRENCE('M4 short cap screw (14):1',
'M4 short cap screw (14):1','M4 short cap screw (14):1',#24261,#24281,
'M4 short cap screw (14):1');
#477=NEXT_ASSEMBLY_USAGE_OCCURRENCE('M4 short cap screw (15):1',
'M4 short cap screw (15):1','M4 short cap screw (15):1',#24261,#24282,
'M4 short cap screw (15):1');
#478=NEXT_ASSEMBLY_USAGE_OCCURRENCE(
'Sealed Ball Bearing - 12 x 32 x 10 mm:2',
'Sealed Ball Bearing - 12 x 32 x 10 mm:2',
'Sealed Ball Bearing - 12 x 32 x 10 mm:2',#24261,#24305,
'Sealed Ball Bearing - 12 x 32 x 10 mm:2');
#479=NEXT_ASSEMBLY_USAGE_OCCURRENCE(
'Sealed Ball Bearing - 12 x 32 x 10 mm:3',
'Sealed Ball Bearing - 12 x 32 x 10 mm:3',
'Sealed Ball Bearing - 12 x 32 x 10 mm:3',#24261,#24305,
'Sealed Ball Bearing - 12 x 32 x 10 mm:3');
#480=NEXT_ASSEMBLY_USAGE_OCCURRENCE('Output link (1):1',
'Output link (1):1','Output link (1):1',#24283,#24284,
'Output link (1):1');
#481=NEXT_ASSEMBLY_USAGE_OCCURRENCE('Bearing cap (4):1',
'Bearing cap (4):1','Bearing cap (4):1',#24283,#24285,
'Bearing cap (4):1');
#482=NEXT_ASSEMBLY_USAGE_OCCURRENCE('M4 short cap screw (16):1',
'M4 short cap screw (16):1','M4 short cap screw (16):1',#24283,#24286,
'M4 short cap screw (16):1');
#483=NEXT_ASSEMBLY_USAGE_OCCURRENCE('M4 short cap screw (17):1',
'M4 short cap screw (17):1','M4 short cap screw (17):1',#24283,#24287,
'M4 short cap screw (17):1');
#484=NEXT_ASSEMBLY_USAGE_OCCURRENCE('M4 short cap screw (18):1',
'M4 short cap screw (18):1','M4 short cap screw (18):1',#24283,#24288,
'M4 short cap screw (18):1');
#485=NEXT_ASSEMBLY_USAGE_OCCURRENCE('M4 short cap screw (19):1',
'M4 short cap screw (19):1','M4 short cap screw (19):1',#24283,#24289,
'M4 short cap screw (19):1');
#486=NEXT_ASSEMBLY_USAGE_OCCURRENCE('Bearing cap (5):1',
'Bearing cap (5):1','Bearing cap (5):1',#24283,#24290,
'Bearing cap (5):1');
#487=NEXT_ASSEMBLY_USAGE_OCCURRENCE('M4 short cap screw (20):1',
'M4 short cap screw (20):1','M4 short cap screw (20):1',#24283,#24291,
'M4 short cap screw (20):1');
#488=NEXT_ASSEMBLY_USAGE_OCCURRENCE('M4 short cap screw (21):1',
'M4 short cap screw (21):1','M4 short cap screw (21):1',#24283,#24292,
'M4 short cap screw (21):1');
#489=NEXT_ASSEMBLY_USAGE_OCCURRENCE('M4 short cap screw (22):1',
'M4 short cap screw (22):1','M4 short cap screw (22):1',#24283,#24293,
'M4 short cap screw (22):1');
#490=NEXT_ASSEMBLY_USAGE_OCCURRENCE('M4 short cap screw (23):1',
'M4 short cap screw (23):1','M4 short cap screw (23):1',#24283,#24294,
'M4 short cap screw (23):1');
#491=NEXT_ASSEMBLY_USAGE_OCCURRENCE('Bearing cap (6):1',
'Bearing cap (6):1','Bearing cap (6):1',#24283,#24295,
'Bearing cap (6):1');
#492=NEXT_ASSEMBLY_USAGE_OCCURRENCE('M4 short cap screw (24):1',
'M4 short cap screw (24):1','M4 short cap screw (24):1',#24283,#24296,
'M4 short cap screw (24):1');
#493=NEXT_ASSEMBLY_USAGE_OCCURRENCE('M4 short cap screw (25):1',
'M4 short cap screw (25):1','M4 short cap screw (25):1',#24283,#24297,
'M4 short cap screw (25):1');
#494=NEXT_ASSEMBLY_USAGE_OCCURRENCE('M4 short cap screw (26):1',
'M4 short cap screw (26):1','M4 short cap screw (26):1',#24283,#24298,
'M4 short cap screw (26):1');
#495=NEXT_ASSEMBLY_USAGE_OCCURRENCE('M4 short cap screw (27):1',
'M4 short cap screw (27):1','M4 short cap screw (27):1',#24283,#24299,
'M4 short cap screw (27):1');
#496=NEXT_ASSEMBLY_USAGE_OCCURRENCE('Bearing cap (7):1',
'Bearing cap (7):1','Bearing cap (7):1',#24283,#24300,
'Bearing cap (7):1');
#497=NEXT_ASSEMBLY_USAGE_OCCURRENCE('M4 short cap screw (28):1',
'M4 short cap screw (28):1','M4 short cap screw (28):1',#24283,#24301,
'M4 short cap screw (28):1');
#498=NEXT_ASSEMBLY_USAGE_OCCURRENCE('M4 short cap screw (29):1',
'M4 short cap screw (29):1','M4 short cap screw (29):1',#24283,#24302,
'M4 short cap screw (29):1');
#499=NEXT_ASSEMBLY_USAGE_OCCURRENCE('M4 short cap screw (30):1',
'M4 short cap screw (30):1','M4 short cap screw (30):1',#24283,#24303,
'M4 short cap screw (30):1');
#500=NEXT_ASSEMBLY_USAGE_OCCURRENCE('M4 short cap screw (31):1',
'M4 short cap screw (31):1','M4 short cap screw (31):1',#24283,#24304,
'M4 short cap screw (31):1');
#501=NEXT_ASSEMBLY_USAGE_OCCURRENCE(
'Sealed Ball Bearing - 12 x 32 x 10 mm:4',
'Sealed Ball Bearing - 12 x 32 x 10 mm:4',
'Sealed Ball Bearing - 12 x 32 x 10 mm:4',#24283,#24305,
'Sealed Ball Bearing - 12 x 32 x 10 mm:4');
#502=NEXT_ASSEMBLY_USAGE_OCCURRENCE(
'Sealed Ball Bearing - 12 x 32 x 10 mm:5',
'Sealed Ball Bearing - 12 x 32 x 10 mm:5',
'Sealed Ball Bearing - 12 x 32 x 10 mm:5',#24283,#24305,
'Sealed Ball Bearing - 12 x 32 x 10 mm:5');
#503=NEXT_ASSEMBLY_USAGE_OCCURRENCE('Base:1','Base:1','Base:1',#24230,#24231,
'Base:1');
#504=NEXT_ASSEMBLY_USAGE_OCCURRENCE('Foot:1','Foot:1','Foot:1',#24230,#24232,
'Foot:1');
#505=NEXT_ASSEMBLY_USAGE_OCCURRENCE('Foot (1):1','Foot (1):1',
'Foot (1):1',#24230,#24233,'Foot (1):1');
#506=NEXT_ASSEMBLY_USAGE_OCCURRENCE('Pivot post:1','Pivot post:1',
'Pivot post:1',#24230,#24234,'Pivot post:1');
#507=NEXT_ASSEMBLY_USAGE_OCCURRENCE('Pivot post (1):1',
'Pivot post (1):1','Pivot post (1):1',#24230,#24235,'Pivot post (1):1');
#508=NEXT_ASSEMBLY_USAGE_OCCURRENCE('Pivot pin:1','Pivot pin:1',
'Pivot pin:1',#24230,#24236,'Pivot pin:1');
#509=NEXT_ASSEMBLY_USAGE_OCCURRENCE('Pivot spacer 36 mm:1',
'Pivot spacer 36 mm:1','Pivot spacer 36 mm:1',#24230,#24237,
'Pivot spacer 36 mm:1');
#510=NEXT_ASSEMBLY_USAGE_OCCURRENCE('Pivot spacer 5 mm:1',
'Pivot spacer 5 mm:1','Pivot spacer 5 mm:1',#24230,#24238,
'Pivot spacer 5 mm:1');
#511=NEXT_ASSEMBLY_USAGE_OCCURRENCE('Pivot keeper:1','Pivot keeper:1',
'Pivot keeper:1',#24230,#24239,'Pivot keeper:1');
#512=NEXT_ASSEMBLY_USAGE_OCCURRENCE('Pivot pin (1):1','Pivot pin (1):1',
'Pivot pin (1):1',#24230,#24240,'Pivot pin (1):1');
#513=NEXT_ASSEMBLY_USAGE_OCCURRENCE('Pivot spacer 36 mm (1):1',
'Pivot spacer 36 mm (1):1','Pivot spacer 36 mm (1):1',#24230,#24241,
'Pivot spacer 36 mm (1):1');
#514=NEXT_ASSEMBLY_USAGE_OCCURRENCE('Pivot spacer 5 mm (1):1',
'Pivot spacer 5 mm (1):1','Pivot spacer 5 mm (1):1',#24230,#24242,
'Pivot spacer 5 mm (1):1');
#515=NEXT_ASSEMBLY_USAGE_OCCURRENCE('Pivot keeper (1):1',
'Pivot keeper (1):1','Pivot keeper (1):1',#24230,#24243,
'Pivot keeper (1):1');
#516=NEXT_ASSEMBLY_USAGE_OCCURRENCE('Screw and guide support:1',
'Screw and guide support:1','Screw and guide support:1',#24230,#24244,
'Screw and guide support:1');
#517=NEXT_ASSEMBLY_USAGE_OCCURRENCE('Screw bearing keeper:1',
'Screw bearing keeper:1','Screw bearing keeper:1',#24230,#24245,
'Screw bearing keeper:1');
#518=NEXT_ASSEMBLY_USAGE_OCCURRENCE('Screw keeper fastener:1',
'Screw keeper fastener:1','Screw keeper fastener:1',#24230,#24246,
'Screw keeper fastener:1');
#519=NEXT_ASSEMBLY_USAGE_OCCURRENCE('Screw keeper fastener (1):1',
'Screw keeper fastener (1):1','Screw keeper fastener (1):1',#24230,#24247,
'Screw keeper fastener (1):1');
#520=NEXT_ASSEMBLY_USAGE_OCCURRENCE('Screw bearing keeper (1):1',
'Screw bearing keeper (1):1','Screw bearing keeper (1):1',#24230,#24248,
'Screw bearing keeper (1):1');
#521=NEXT_ASSEMBLY_USAGE_OCCURRENCE('Screw keeper fastener (2):1',
'Screw keeper fastener (2):1','Screw keeper fastener (2):1',#24230,#24249,
'Screw keeper fastener (2):1');
#522=NEXT_ASSEMBLY_USAGE_OCCURRENCE('Screw keeper fastener (3):1',
'Screw keeper fastener (3):1','Screw keeper fastener (3):1',#24230,#24250,
'Screw keeper fastener (3):1');
#523=NEXT_ASSEMBLY_USAGE_OCCURRENCE('Screw and guide support (1):1',
'Screw and guide support (1):1','Screw and guide support (1):1',#24230,
#24251,'Screw and guide support (1):1');
#524=NEXT_ASSEMBLY_USAGE_OCCURRENCE('Screw bearing keeper (2):1',
'Screw bearing keeper (2):1','Screw bearing keeper (2):1',#24230,#24252,
'Screw bearing keeper (2):1');
#525=NEXT_ASSEMBLY_USAGE_OCCURRENCE('Screw keeper fastener (4):1',
'Screw keeper fastener (4):1','Screw keeper fastener (4):1',#24230,#24253,
'Screw keeper fastener (4):1');
#526=NEXT_ASSEMBLY_USAGE_OCCURRENCE('Screw keeper fastener (5):1',
'Screw keeper fastener (5):1','Screw keeper fastener (5):1',#24230,#24254,
'Screw keeper fastener (5):1');
#527=NEXT_ASSEMBLY_USAGE_OCCURRENCE('Screw bearing keeper (3):1',
'Screw bearing keeper (3):1','Screw bearing keeper (3):1',#24230,#24255,
'Screw bearing keeper (3):1');
#528=NEXT_ASSEMBLY_USAGE_OCCURRENCE('Screw keeper fastener (6):1',
'Screw keeper fastener (6):1','Screw keeper fastener (6):1',#24230,#24256,
'Screw keeper fastener (6):1');
#529=NEXT_ASSEMBLY_USAGE_OCCURRENCE('Screw keeper fastener (7):1',
'Screw keeper fastener (7):1','Screw keeper fastener (7):1',#24230,#24257,
'Screw keeper fastener (7):1');
#530=NEXT_ASSEMBLY_USAGE_OCCURRENCE('Guide shaft:1','Guide shaft:1',
'Guide shaft:1',#24230,#24258,'Guide shaft:1');
#531=NEXT_ASSEMBLY_USAGE_OCCURRENCE('Guide shaft (1):1',
'Guide shaft (1):1','Guide shaft (1):1',#24230,#24259,
'Guide shaft (1):1');
#532=NEXT_ASSEMBLY_USAGE_OCCURRENCE('Cap Screw - M5x20:2',
'Cap Screw - M5x20:2','Cap Screw - M5x20:2',#24230,#24260,
'Cap Screw - M5x20:2');
#533=NEXT_ASSEMBLY_USAGE_OCCURRENCE('Cap Screw - M5x20:3',
'Cap Screw - M5x20:3','Cap Screw - M5x20:3',#24230,#24260,
'Cap Screw - M5x20:3');
#534=NEXT_ASSEMBLY_USAGE_OCCURRENCE('Cap Screw - M5x20:4',
'Cap Screw - M5x20:4','Cap Screw - M5x20:4',#24230,#24260,
'Cap Screw - M5x20:4');
#535=NEXT_ASSEMBLY_USAGE_OCCURRENCE('Cap Screw - M5x20:5',
'Cap Screw - M5x20:5','Cap Screw - M5x20:5',#24230,#24260,
'Cap Screw - M5x20:5');
#536=NEXT_ASSEMBLY_USAGE_OCCURRENCE('Cap Screw - M5x20:6',
'Cap Screw - M5x20:6','Cap Screw - M5x20:6',#24230,#24260,
'Cap Screw - M5x20:6');
#537=NEXT_ASSEMBLY_USAGE_OCCURRENCE('Cap Screw - M5x20:7',
'Cap Screw - M5x20:7','Cap Screw - M5x20:7',#24230,#24260,
'Cap Screw - M5x20:7');
#538=NEXT_ASSEMBLY_USAGE_OCCURRENCE('Cap Screw - M5x20:8',
'Cap Screw - M5x20:8','Cap Screw - M5x20:8',#24230,#24260,
'Cap Screw - M5x20:8');
#539=NEXT_ASSEMBLY_USAGE_OCCURRENCE('Cap Screw - M5x20:9',
'Cap Screw - M5x20:9','Cap Screw - M5x20:9',#24230,#24260,
'Cap Screw - M5x20:9');
#540=NEXT_ASSEMBLY_USAGE_OCCURRENCE('Cap Screw - M4x16:2',
'Cap Screw - M4x16:2','Cap Screw - M4x16:2',#24230,#24324,
'Cap Screw - M4x16:2');
#541=NEXT_ASSEMBLY_USAGE_OCCURRENCE('Cap Screw - M4x16:3',
'Cap Screw - M4x16:3','Cap Screw - M4x16:3',#24230,#24324,
'Cap Screw - M4x16:3');
#542=NEXT_ASSEMBLY_USAGE_OCCURRENCE('Cap Screw - M4x16:4',
'Cap Screw - M4x16:4','Cap Screw - M4x16:4',#24230,#24324,
'Cap Screw - M4x16:4');
#543=NEXT_ASSEMBLY_USAGE_OCCURRENCE('Cap Screw - M4x16:5',
'Cap Screw - M4x16:5','Cap Screw - M4x16:5',#24230,#24324,
'Cap Screw - M4x16:5');
#544=NEXT_ASSEMBLY_USAGE_OCCURRENCE('Cap Screw - M4x16:10',
'Cap Screw - M4x16:10','Cap Screw - M4x16:10',#24230,#24324,
'Cap Screw - M4x16:10');
#545=NEXT_ASSEMBLY_USAGE_OCCURRENCE('Cap Screw - M4x16:11',
'Cap Screw - M4x16:11','Cap Screw - M4x16:11',#24230,#24324,
'Cap Screw - M4x16:11');
#546=NEXT_ASSEMBLY_USAGE_OCCURRENCE('Cap Screw - M4x16:12',
'Cap Screw - M4x16:12','Cap Screw - M4x16:12',#24230,#24324,
'Cap Screw - M4x16:12');
#547=NEXT_ASSEMBLY_USAGE_OCCURRENCE('Cap Screw - M4x16:13',
'Cap Screw - M4x16:13','Cap Screw - M4x16:13',#24230,#24324,
'Cap Screw - M4x16:13');
#548=NEXT_ASSEMBLY_USAGE_OCCURRENCE(
'Sealed Ball Bearing - 12 x 32 x 10 mm:6',
'Sealed Ball Bearing - 12 x 32 x 10 mm:6',
'Sealed Ball Bearing - 12 x 32 x 10 mm:6',#24230,#24305,
'Sealed Ball Bearing - 12 x 32 x 10 mm:6');
#549=NEXT_ASSEMBLY_USAGE_OCCURRENCE('Cap Screw - M4x16:18',
'Cap Screw - M4x16:18','Cap Screw - M4x16:18',#24230,#24324,
'Cap Screw - M4x16:18');
#550=NEXT_ASSEMBLY_USAGE_OCCURRENCE('Cap Screw - M4x16:19',
'Cap Screw - M4x16:19','Cap Screw - M4x16:19',#24230,#24324,
'Cap Screw - M4x16:19');
#551=NEXT_ASSEMBLY_USAGE_OCCURRENCE(
'Sealed Ball Bearing - 12 x 32 x 10 mm:7',
'Sealed Ball Bearing - 12 x 32 x 10 mm:7',
'Sealed Ball Bearing - 12 x 32 x 10 mm:7',#24230,#24305,
'Sealed Ball Bearing - 12 x 32 x 10 mm:7');
#552=NEXT_ASSEMBLY_USAGE_OCCURRENCE('Cap Screw - M4x16:20',
'Cap Screw - M4x16:20','Cap Screw - M4x16:20',#24230,#24324,
'Cap Screw - M4x16:20');
#553=NEXT_ASSEMBLY_USAGE_OCCURRENCE('Cap Screw - M4x16:21',
'Cap Screw - M4x16:21','Cap Screw - M4x16:21',#24230,#24324,
'Cap Screw - M4x16:21');
#554=NEXT_ASSEMBLY_USAGE_OCCURRENCE('Cradle frame:1','Cradle frame:1',
'Cradle frame:1',#24311,#24312,'Cradle frame:1');
#555=NEXT_ASSEMBLY_USAGE_OCCURRENCE('Cradle rim:1','Cradle rim:1',
'Cradle rim:1',#24311,#24313,'Cradle rim:1');
#556=NEXT_ASSEMBLY_USAGE_OCCURRENCE('Cradle rim (1):1',
'Cradle rim (1):1','Cradle rim (1):1',#24311,#24314,'Cradle rim (1):1');
#557=NEXT_ASSEMBLY_USAGE_OCCURRENCE('Actuator pivot pin:1',
'Actuator pivot pin:1','Actuator pivot pin:1',#24311,#24315,
'Actuator pivot pin:1');
#558=NEXT_ASSEMBLY_USAGE_OCCURRENCE('Pivot spacer 16 mm:1',
'Pivot spacer 16 mm:1','Pivot spacer 16 mm:1',#24311,#24316,
'Pivot spacer 16 mm:1');
#559=NEXT_ASSEMBLY_USAGE_OCCURRENCE('Pivot spacer 35 mm:1',
'Pivot spacer 35 mm:1','Pivot spacer 35 mm:1',#24311,#24317,
'Pivot spacer 35 mm:1');
#560=NEXT_ASSEMBLY_USAGE_OCCURRENCE('Pivot spacer 5 mm (2):1',
'Pivot spacer 5 mm (2):1','Pivot spacer 5 mm (2):1',#24311,#24318,
'Pivot spacer 5 mm (2):1');
#561=NEXT_ASSEMBLY_USAGE_OCCURRENCE('Pivot keeper (2):1',
'Pivot keeper (2):1','Pivot keeper (2):1',#24311,#24319,
'Pivot keeper (2):1');
#562=NEXT_ASSEMBLY_USAGE_OCCURRENCE('Pivot pin (2):1','Pivot pin (2):1',
'Pivot pin (2):1',#24311,#24320,'Pivot pin (2):1');
#563=NEXT_ASSEMBLY_USAGE_OCCURRENCE('Pivot spacer 16 mm (1):1',
'Pivot spacer 16 mm (1):1','Pivot spacer 16 mm (1):1',#24311,#24321,
'Pivot spacer 16 mm (1):1');
#564=NEXT_ASSEMBLY_USAGE_OCCURRENCE('Pivot spacer 5 mm (3):1',
'Pivot spacer 5 mm (3):1','Pivot spacer 5 mm (3):1',#24311,#24322,
'Pivot spacer 5 mm (3):1');
#565=NEXT_ASSEMBLY_USAGE_OCCURRENCE('Pivot keeper (3):1',
'Pivot keeper (3):1','Pivot keeper (3):1',#24311,#24323,
'Pivot keeper (3):1');
#566=NEXT_ASSEMBLY_USAGE_OCCURRENCE('Cap Screw - M4x16:6',
'Cap Screw - M4x16:6','Cap Screw - M4x16:6',#24311,#24324,
'Cap Screw - M4x16:6');
#567=NEXT_ASSEMBLY_USAGE_OCCURRENCE('Cap Screw - M4x16:7',
'Cap Screw - M4x16:7','Cap Screw - M4x16:7',#24311,#24324,
'Cap Screw - M4x16:7');
#568=NEXT_ASSEMBLY_USAGE_OCCURRENCE('Cap Screw - M4x16:8',
'Cap Screw - M4x16:8','Cap Screw - M4x16:8',#24311,#24324,
'Cap Screw - M4x16:8');
#569=NEXT_ASSEMBLY_USAGE_OCCURRENCE('Cap Screw - M4x16:9',
'Cap Screw - M4x16:9','Cap Screw - M4x16:9',#24311,#24324,
'Cap Screw - M4x16:9');
#570=NEXT_ASSEMBLY_USAGE_OCCURRENCE('Cap Screw - M4x16:14',
'Cap Screw - M4x16:14','Cap Screw - M4x16:14',#24311,#24324,
'Cap Screw - M4x16:14');
#571=NEXT_ASSEMBLY_USAGE_OCCURRENCE('Cap Screw - M4x16:15',
'Cap Screw - M4x16:15','Cap Screw - M4x16:15',#24311,#24324,
'Cap Screw - M4x16:15');
#572=NEXT_ASSEMBLY_USAGE_OCCURRENCE('Cap Screw - M4x16:16',
'Cap Screw - M4x16:16','Cap Screw - M4x16:16',#24311,#24324,
'Cap Screw - M4x16:16');
#573=NEXT_ASSEMBLY_USAGE_OCCURRENCE('Cap Screw - M4x16:17',
'Cap Screw - M4x16:17','Cap Screw - M4x16:17',#24311,#24324,
'Cap Screw - M4x16:17');
#574=NEXT_ASSEMBLY_USAGE_OCCURRENCE('Steel sleeve:1','Steel sleeve:1',
'Steel sleeve:1',#24333,#24334,'Steel sleeve:1');
#575=NEXT_ASSEMBLY_USAGE_OCCURRENCE('Ball retainer (plastic):1',
'Ball retainer (plastic):1','Ball retainer (plastic):1',#24333,#24335,
'Ball retainer (plastic):1');
#576=NEXT_ASSEMBLY_USAGE_OCCURRENCE('Nut carriage:1','Nut carriage:1',
'Nut carriage:1',#24325,#24326,'Nut carriage:1');
#577=NEXT_ASSEMBLY_USAGE_OCCURRENCE('Guide bearing retainer:1',
'Guide bearing retainer:1','Guide bearing retainer:1',#24325,#24327,
'Guide bearing retainer:1');
#578=NEXT_ASSEMBLY_USAGE_OCCURRENCE('Guide bearing retainer (1):1',
'Guide bearing retainer (1):1','Guide bearing retainer (1):1',#24325,#24328,
'Guide bearing retainer (1):1');
#579=NEXT_ASSEMBLY_USAGE_OCCURRENCE('Connecting link clevis:1',
'Connecting link clevis:1','Connecting link clevis:1',#24325,#24329,
'Connecting link clevis:1');
#580=NEXT_ASSEMBLY_USAGE_OCCURRENCE('Actuator clevis pin:1',
'Actuator clevis pin:1','Actuator clevis pin:1',#24325,#24330,
'Actuator clevis pin:1');
#581=NEXT_ASSEMBLY_USAGE_OCCURRENCE('Actuator pin keeper:1',
'Actuator pin keeper:1','Actuator pin keeper:1',#24325,#24331,
'Actuator pin keeper:1');
#582=NEXT_ASSEMBLY_USAGE_OCCURRENCE('Actuator pin spacer:1',
'Actuator pin spacer:1','Actuator pin spacer:1',#24325,#24332,
'Actuator pin spacer:1');
#583=NEXT_ASSEMBLY_USAGE_OCCURRENCE(
'Linear Ball Bushing - 12 x 21 x 30 mm:2',
'Linear Ball Bushing - 12 x 21 x 30 mm:2',
'Linear Ball Bushing - 12 x 21 x 30 mm:2',#24325,#24333,
'Linear Ball Bushing - 12 x 21 x 30 mm:2');
#584=NEXT_ASSEMBLY_USAGE_OCCURRENCE(
'Linear Ball Bushing - 12 x 21 x 30 mm:3',
'Linear Ball Bushing - 12 x 21 x 30 mm:3',
'Linear Ball Bushing - 12 x 21 x 30 mm:3',#24325,#24333,
'Linear Ball Bushing - 12 x 21 x 30 mm:3');
#585=NEXT_ASSEMBLY_USAGE_OCCURRENCE('M4x10 Cap Screw:2',
'M4x10 Cap Screw:2','M4x10 Cap Screw:2',#24325,#24336,
'M4x10 Cap Screw:2');
#586=NEXT_ASSEMBLY_USAGE_OCCURRENCE('Actuator link:1','Actuator link:1',
'Actuator link:1',#24337,#24338,'Actuator link:1');
#587=NEXT_ASSEMBLY_USAGE_OCCURRENCE('Feed screw:1','Feed screw:1',
'Feed screw:1',#24339,#24340,'Feed screw:1');
#588=NEXT_ASSEMBLY_USAGE_OCCURRENCE('Screw thrust collar:1',
'Screw thrust collar:1','Screw thrust collar:1',#24339,#24341,
'Screw thrust collar:1');
#589=NEXT_ASSEMBLY_USAGE_OCCURRENCE('Screw thrust collar (1):1',
'Screw thrust collar (1):1','Screw thrust collar (1):1',#24339,#24342,
'Screw thrust collar (1):1');
#590=NEXT_ASSEMBLY_USAGE_OCCURRENCE('Handwheel:1','Handwheel:1',
'Handwheel:1',#24339,#24343,'Handwheel:1');
#591=NEXT_ASSEMBLY_USAGE_OCCURRENCE('Handwheel grip:1',
'Handwheel grip:1','Handwheel grip:1',#24339,#24344,'Handwheel grip:1');
#592=NEXT_ASSEMBLY_USAGE_OCCURRENCE('Base and pivots:1',
'Base and pivots:1','Base and pivots:1',#24229,#24230,
'Base and pivots:1');
#593=NEXT_ASSEMBLY_USAGE_OCCURRENCE('Input link:1','Input link:1',
'Input link:1',#24229,#24261,'Input link:1');
#594=NEXT_ASSEMBLY_USAGE_OCCURRENCE('Output link:1','Output link:1',
'Output link:1',#24229,#24283,'Output link:1');
#595=NEXT_ASSEMBLY_USAGE_OCCURRENCE('Tilting cradle:1',
'Tilting cradle:1','Tilting cradle:1',#24229,#24311,'Tilting cradle:1');
#596=NEXT_ASSEMBLY_USAGE_OCCURRENCE('Traveling nut:1','Traveling nut:1',
'Traveling nut:1',#24229,#24325,'Traveling nut:1');
#597=NEXT_ASSEMBLY_USAGE_OCCURRENCE('Actuator connecting link:1',
'Actuator connecting link:1','Actuator connecting link:1',#24229,#24337,
'Actuator connecting link:1');
#598=NEXT_ASSEMBLY_USAGE_OCCURRENCE('Feed screw and handwheel:1',
'Feed screw and handwheel:1','Feed screw and handwheel:1',#24229,#24339,
'Feed screw and handwheel:1');
#599=B_SPLINE_CURVE_WITH_KNOTS('',3,(#21962,#21963,#21964,#21965,#21966,
#21967,#21968,#21969,#21970,#21971,#21972,#21973,#21974,#21975,#21976,#21977,
#21978,#21979,#21980,#21981,#21982,#21983),.UNSPECIFIED.,.F.,.F.,(4,2,2,
2,2,2,2,2,2,2,4),(0.0591825211272536,0.157966726598481,0.236950089897721,
0.315933453196962,0.391576304923761,0.46721915665056,0.54286200837736,0.618504860104159,
0.697488223403399,0.77647158670264,0.875255792173867),.UNSPECIFIED.);
#600=B_SPLINE_CURVE_WITH_KNOTS('',3,(#21987,#21988,#21989,#21990,#21991,
#21992,#21993,#21994,#21995,#21996,#21997,#21998,#21999,#22000,#22001,#22002,
#22003,#22004,#22005,#22006,#22007,#22008),.UNSPECIFIED.,.F.,.F.,(4,2,2,
2,2,2,2,2,2,2,4),(0.0581119756758434,0.106553146291161,0.213106292582322,
0.30849933801665,0.386091982889075,0.4636846277615,0.541277272633925,0.61886991750635,
0.714262962940678,0.820816109231839,0.869257279847157),.UNSPECIFIED.);
#601=B_SPLINE_CURVE_WITH_KNOTS('',3,(#22014,#22015,#22016,#22017,#22018,
#22019,#22020,#22021,#22022,#22023,#22024,#22025,#22026,#22027,#22028,#22029,
#22030,#22031,#22032,#22033,#22034,#22035),.UNSPECIFIED.,.F.,.F.,(4,2,2,
2,2,2,2,2,2,2,4),(0.0581119756758434,0.106553146291161,0.213106292582322,
0.30849933801665,0.386091982889075,0.4636846277615,0.541277272633925,0.61886991750635,
0.714262962940679,0.820816109231839,0.869257279847157),.UNSPECIFIED.);
#602=B_SPLINE_CURVE_WITH_KNOTS('',3,(#22039,#22040,#22041,#22042,#22043,
#22044,#22045,#22046,#22047,#22048,#22049,#22050,#22051,#22052,#22053,#22054,
#22055,#22056,#22057,#22058,#22059,#22060),.UNSPECIFIED.,.F.,.F.,(4,2,2,
2,2,2,2,2,2,2,4),(0.0581119756758433,0.106553146291161,0.213106292582322,
0.308499338016649,0.386091982889075,0.4636846277615,0.541277272633925,0.61886991750635,
0.714262962940678,0.820816109231839,0.869257279847157),.UNSPECIFIED.);
#603=B_SPLINE_CURVE_WITH_KNOTS('',3,(#22069,#22070,#22071,#22072,#22073,
#22074,#22075,#22076,#22077,#22078,#22079,#22080,#22081,#22082,#22083,#22084,
#22085,#22086,#22087,#22088,#22089,#22090),.UNSPECIFIED.,.F.,.F.,(4,2,2,
2,2,2,2,2,2,2,4),(0.0581119756758433,0.106553146291161,0.213106292582322,
0.30849933801665,0.386091982889075,0.4636846277615,0.541277272633925,0.61886991750635,
0.714262962940678,0.820816109231839,0.869257279847157),.UNSPECIFIED.);
#604=B_SPLINE_CURVE_WITH_KNOTS('',3,(#22094,#22095,#22096,#22097,#22098,
#22099,#22100,#22101,#22102,#22103,#22104,#22105,#22106,#22107,#22108,#22109,
#22110,#22111,#22112,#22113,#22114,#22115),.UNSPECIFIED.,.F.,.F.,(4,2,2,
2,2,2,2,2,2,2,4),(0.0581119756758434,0.106553146291161,0.213106292582322,
0.30849933801665,0.386091982889075,0.4636846277615,0.541277272633925,0.61886991750635,
0.714262962940678,0.820816109231839,0.869257279847157),.UNSPECIFIED.);
#605=B_SPLINE_CURVE_WITH_KNOTS('',3,(#22119,#22120,#22121,#22122,#22123,
#22124,#22125,#22126,#22127,#22128,#22129,#22130,#22131,#22132,#22133,#22134,
#22135,#22136,#22137,#22138,#22139,#22140),.UNSPECIFIED.,.F.,.F.,(4,2,2,
2,2,2,2,2,2,2,4),(0.0581119756758434,0.106553146291161,0.213106292582322,
0.30849933801665,0.386091982889075,0.4636846277615,0.541277272633925,0.61886991750635,
0.714262962940678,0.820816109231839,0.869257279847157),.UNSPECIFIED.);
#606=B_SPLINE_CURVE_WITH_KNOTS('',3,(#22144,#22145,#22146,#22147,#22148,
#22149,#22150,#22151,#22152,#22153,#22154,#22155,#22156,#22157,#22158,#22159,
#22160,#22161,#22162,#22163,#22164,#22165),.UNSPECIFIED.,.F.,.F.,(4,2,2,
2,2,2,2,2,2,2,4),(0.0581119756758433,0.106553146291161,0.213106292582322,
0.30849933801665,0.386091982889075,0.4636846277615,0.541277272633925,0.61886991750635,
0.714262962940678,0.820816109231839,0.869257279847157),.UNSPECIFIED.);
#607=B_SPLINE_CURVE_WITH_KNOTS('',3,(#22173,#22174,#22175,#22176,#22177,
#22178,#22179,#22180,#22181,#22182,#22183,#22184,#22185,#22186,#22187,#22188,
#22189,#22190,#22191,#22192,#22193,#22194),.UNSPECIFIED.,.F.,.F.,(4,2,2,
2,2,2,2,2,2,2,4),(0.0591825211272536,0.157966726598481,0.236950089897721,
0.315933453196962,0.391576304923761,0.467219156650561,0.54286200837736,
0.618504860104159,0.697488223403399,0.77647158670264,0.875255792173867),
 .UNSPECIFIED.);
#608=B_SPLINE_CURVE_WITH_KNOTS('',3,(#22202,#22203,#22204,#22205,#22206,
#22207,#22208,#22209,#22210,#22211,#22212,#22213,#22214,#22215,#22216,#22217,
#22218,#22219,#22220,#22221,#22222,#22223),.UNSPECIFIED.,.F.,.F.,(4,2,2,
2,2,2,2,2,2,2,4),(0.0591825211272536,0.157966726598481,0.236950089897722,
0.315933453196962,0.391576304923761,0.467219156650561,0.54286200837736,
0.618504860104159,0.697488223403399,0.77647158670264,0.875255792173867),
 .UNSPECIFIED.);
#609=B_SPLINE_CURVE_WITH_KNOTS('',3,(#22233,#22234,#22235,#22236,#22237,
#22238,#22239,#22240,#22241,#22242,#22243,#22244,#22245,#22246,#22247,#22248,
#22249,#22250,#22251,#22252,#22253,#22254),.UNSPECIFIED.,.F.,.F.,(4,2,2,
2,2,2,2,2,2,2,4),(0.0591825211272536,0.157966726598481,0.236950089897721,
0.315933453196962,0.391576304923761,0.46721915665056,0.54286200837736,0.618504860104159,
0.697488223403399,0.77647158670264,0.875255792173867),.UNSPECIFIED.);
#610=B_SPLINE_CURVE_WITH_KNOTS('',3,(#22262,#22263,#22264,#22265,#22266,
#22267,#22268,#22269,#22270,#22271,#22272,#22273,#22274,#22275,#22276,#22277,
#22278,#22279,#22280,#22281,#22282,#22283),.UNSPECIFIED.,.F.,.F.,(4,2,2,
2,2,2,2,2,2,2,4),(0.0591825211272536,0.157966726598481,0.236950089897721,
0.315933453196962,0.391576304923761,0.46721915665056,0.542862008377359,
0.618504860104159,0.697488223403399,0.776471586702639,0.875255792173867),
 .UNSPECIFIED.);
#611=B_SPLINE_CURVE_WITH_KNOTS('',3,(#22291,#22292,#22293,#22294,#22295,
#22296,#22297,#22298,#22299,#22300,#22301,#22302,#22303,#22304,#22305,#22306,
#22307,#22308,#22309,#22310,#22311,#22312),.UNSPECIFIED.,.F.,.F.,(4,2,2,
2,2,2,2,2,2,2,4),(0.0591825211272536,0.157966726598481,0.236950089897721,
0.315933453196962,0.391576304923761,0.46721915665056,0.54286200837736,0.618504860104159,
0.697488223403399,0.77647158670264,0.875255792173867),.UNSPECIFIED.);
#612=B_SPLINE_CURVE_WITH_KNOTS('',3,(#22321,#22322,#22323,#22324,#22325,
#22326,#22327,#22328,#22329,#22330,#22331,#22332,#22333,#22334,#22335,#22336,
#22337,#22338,#22339,#22340,#22341,#22342),.UNSPECIFIED.,.F.,.F.,(4,2,2,
2,2,2,2,2,2,2,4),(0.0591825211272536,0.157966726598481,0.236950089897721,
0.315933453196962,0.391576304923761,0.46721915665056,0.542862008377359,
0.618504860104159,0.697488223403399,0.776471586702639,0.875255792173867),
 .UNSPECIFIED.);
#613=SPHERICAL_SURFACE('',#14815,0.29765);
#614=SPHERICAL_SURFACE('',#14817,0.29765);
#615=SPHERICAL_SURFACE('',#14819,0.29765);
#616=SPHERICAL_SURFACE('',#14821,0.29765);
#617=SPHERICAL_SURFACE('',#14823,0.29765);
#618=SPHERICAL_SURFACE('',#14825,0.29765);
#619=SPHERICAL_SURFACE('',#14827,0.29765);
#620=SPHERICAL_SURFACE('',#14830,0.309556);
#621=SPHERICAL_SURFACE('',#14846,0.309556);
#622=SPHERICAL_SURFACE('',#14851,0.309556);
#623=SPHERICAL_SURFACE('',#14857,0.309556);
#624=SPHERICAL_SURFACE('',#14862,0.309556);
#625=SPHERICAL_SURFACE('',#14867,0.309556);
#626=SPHERICAL_SURFACE('',#14875,0.309556);
#627=TOROIDAL_SURFACE('',#14775,1.1,0.309556);
#628=TOROIDAL_SURFACE('',#14795,1.1,0.309556);
#629=ORIENTED_CLOSED_SHELL('',*,#12422,.F.);
#630=ORIENTED_CLOSED_SHELL('',*,#12491,.F.);
#631=ORIENTED_CLOSED_SHELL('',*,#12501,.F.);
#632=CONICAL_SURFACE('',#14178,0.4,0.785398163397448);
#633=CONICAL_SURFACE('',#14182,0.41,0.785398163397448);
#634=CONICAL_SURFACE('',#14186,0.26,0.463647609000806);
#635=CONICAL_SURFACE('',#14190,0.225,0.785398163397448);
#636=CONICAL_SURFACE('',#14786,0.63,0.785398163397448);
#637=CONICAL_SURFACE('',#14793,0.63,0.785398163397448);
#638=CONICAL_SURFACE('',#14806,1.57,0.785398163397449);
#639=CONICAL_SURFACE('',#14810,1.57,0.785398163397449);
#640=CONICAL_SURFACE('',#15132,0.325,0.785398163397448);
#641=CONICAL_SURFACE('',#15136,0.335,0.785398163397448);
#642=CONICAL_SURFACE('',#15140,0.21,0.463647609000806);
#643=CONICAL_SURFACE('',#15144,0.18,0.785398163397448);
#644=CONICAL_SURFACE('',#15382,0.325,0.785398163397448);
#645=CONICAL_SURFACE('',#15386,0.335,0.785398163397448);
#646=CONICAL_SURFACE('',#15390,0.21,0.463647609000806);
#647=BREP_WITH_VOIDS('Body1',#12421,(#629));
#648=BREP_WITH_VOIDS('Body1',#12490,(#630));
#649=BREP_WITH_VOIDS('Body1',#12502,(#631));
#650=SHAPE_REPRESENTATION_RELATIONSHIP('SRR','None',#24114,#756);
#651=SHAPE_REPRESENTATION_RELATIONSHIP('SRR','None',#24115,#757);
#652=SHAPE_REPRESENTATION_RELATIONSHIP('SRR','None',#24116,#758);
#653=SHAPE_REPRESENTATION_RELATIONSHIP('SRR','None',#24117,#759);
#654=SHAPE_REPRESENTATION_RELATIONSHIP('SRR','None',#24118,#760);
#655=SHAPE_REPRESENTATION_RELATIONSHIP('SRR','None',#24119,#761);
#656=SHAPE_REPRESENTATION_RELATIONSHIP('SRR','None',#24120,#762);
#657=SHAPE_REPRESENTATION_RELATIONSHIP('SRR','None',#24121,#763);
#658=SHAPE_REPRESENTATION_RELATIONSHIP('SRR','None',#24122,#764);
#659=SHAPE_REPRESENTATION_RELATIONSHIP('SRR','None',#24123,#765);
#660=SHAPE_REPRESENTATION_RELATIONSHIP('SRR','None',#24124,#766);
#661=SHAPE_REPRESENTATION_RELATIONSHIP('SRR','None',#24125,#767);
#662=SHAPE_REPRESENTATION_RELATIONSHIP('SRR','None',#24126,#768);
#663=SHAPE_REPRESENTATION_RELATIONSHIP('SRR','None',#24127,#769);
#664=SHAPE_REPRESENTATION_RELATIONSHIP('SRR','None',#24128,#770);
#665=SHAPE_REPRESENTATION_RELATIONSHIP('SRR','None',#24129,#771);
#666=SHAPE_REPRESENTATION_RELATIONSHIP('SRR','None',#24130,#772);
#667=SHAPE_REPRESENTATION_RELATIONSHIP('SRR','None',#24131,#773);
#668=SHAPE_REPRESENTATION_RELATIONSHIP('SRR','None',#24132,#774);
#669=SHAPE_REPRESENTATION_RELATIONSHIP('SRR','None',#24133,#775);
#670=SHAPE_REPRESENTATION_RELATIONSHIP('SRR','None',#24134,#776);
#671=SHAPE_REPRESENTATION_RELATIONSHIP('SRR','None',#24135,#777);
#672=SHAPE_REPRESENTATION_RELATIONSHIP('SRR','None',#24136,#778);
#673=SHAPE_REPRESENTATION_RELATIONSHIP('SRR','None',#24137,#779);
#674=SHAPE_REPRESENTATION_RELATIONSHIP('SRR','None',#24138,#780);
#675=SHAPE_REPRESENTATION_RELATIONSHIP('SRR','None',#24139,#781);
#676=SHAPE_REPRESENTATION_RELATIONSHIP('SRR','None',#24140,#782);
#677=SHAPE_REPRESENTATION_RELATIONSHIP('SRR','None',#24141,#783);
#678=SHAPE_REPRESENTATION_RELATIONSHIP('SRR','None',#24142,#784);
#679=SHAPE_REPRESENTATION_RELATIONSHIP('SRR','None',#24143,#785);
#680=SHAPE_REPRESENTATION_RELATIONSHIP('SRR','None',#24145,#786);
#681=SHAPE_REPRESENTATION_RELATIONSHIP('SRR','None',#24146,#787);
#682=SHAPE_REPRESENTATION_RELATIONSHIP('SRR','None',#24147,#788);
#683=SHAPE_REPRESENTATION_RELATIONSHIP('SRR','None',#24148,#789);
#684=SHAPE_REPRESENTATION_RELATIONSHIP('SRR','None',#24149,#790);
#685=SHAPE_REPRESENTATION_RELATIONSHIP('SRR','None',#24150,#791);
#686=SHAPE_REPRESENTATION_RELATIONSHIP('SRR','None',#24151,#792);
#687=SHAPE_REPRESENTATION_RELATIONSHIP('SRR','None',#24152,#793);
#688=SHAPE_REPRESENTATION_RELATIONSHIP('SRR','None',#24153,#794);
#689=SHAPE_REPRESENTATION_RELATIONSHIP('SRR','None',#24154,#795);
#690=SHAPE_REPRESENTATION_RELATIONSHIP('SRR','None',#24155,#796);
#691=SHAPE_REPRESENTATION_RELATIONSHIP('SRR','None',#24156,#797);
#692=SHAPE_REPRESENTATION_RELATIONSHIP('SRR','None',#24157,#798);
#693=SHAPE_REPRESENTATION_RELATIONSHIP('SRR','None',#24158,#799);
#694=SHAPE_REPRESENTATION_RELATIONSHIP('SRR','None',#24159,#800);
#695=SHAPE_REPRESENTATION_RELATIONSHIP('SRR','None',#24160,#801);
#696=SHAPE_REPRESENTATION_RELATIONSHIP('SRR','None',#24161,#802);
#697=SHAPE_REPRESENTATION_RELATIONSHIP('SRR','None',#24162,#803);
#698=SHAPE_REPRESENTATION_RELATIONSHIP('SRR','None',#24163,#804);
#699=SHAPE_REPRESENTATION_RELATIONSHIP('SRR','None',#24164,#805);
#700=SHAPE_REPRESENTATION_RELATIONSHIP('SRR','None',#24165,#806);
#701=SHAPE_REPRESENTATION_RELATIONSHIP('SRR','None',#24167,#807);
#702=SHAPE_REPRESENTATION_RELATIONSHIP('SRR','None',#24168,#808);
#703=SHAPE_REPRESENTATION_RELATIONSHIP('SRR','None',#24169,#809);
#704=SHAPE_REPRESENTATION_RELATIONSHIP('SRR','None',#24170,#810);
#705=SHAPE_REPRESENTATION_RELATIONSHIP('SRR','None',#24171,#811);
#706=SHAPE_REPRESENTATION_RELATIONSHIP('SRR','None',#24172,#812);
#707=SHAPE_REPRESENTATION_RELATIONSHIP('SRR','None',#24173,#813);
#708=SHAPE_REPRESENTATION_RELATIONSHIP('SRR','None',#24174,#814);
#709=SHAPE_REPRESENTATION_RELATIONSHIP('SRR','None',#24175,#815);
#710=SHAPE_REPRESENTATION_RELATIONSHIP('SRR','None',#24176,#816);
#711=SHAPE_REPRESENTATION_RELATIONSHIP('SRR','None',#24177,#817);
#712=SHAPE_REPRESENTATION_RELATIONSHIP('SRR','None',#24178,#818);
#713=SHAPE_REPRESENTATION_RELATIONSHIP('SRR','None',#24179,#819);
#714=SHAPE_REPRESENTATION_RELATIONSHIP('SRR','None',#24180,#820);
#715=SHAPE_REPRESENTATION_RELATIONSHIP('SRR','None',#24181,#821);
#716=SHAPE_REPRESENTATION_RELATIONSHIP('SRR','None',#24182,#822);
#717=SHAPE_REPRESENTATION_RELATIONSHIP('SRR','None',#24183,#823);
#718=SHAPE_REPRESENTATION_RELATIONSHIP('SRR','None',#24184,#824);
#719=SHAPE_REPRESENTATION_RELATIONSHIP('SRR','None',#24185,#825);
#720=SHAPE_REPRESENTATION_RELATIONSHIP('SRR','None',#24186,#826);
#721=SHAPE_REPRESENTATION_RELATIONSHIP('SRR','None',#24187,#827);
#722=SHAPE_REPRESENTATION_RELATIONSHIP('SRR','None',#24189,#828);
#723=SHAPE_REPRESENTATION_RELATIONSHIP('SRR','None',#24190,#829);
#724=SHAPE_REPRESENTATION_RELATIONSHIP('SRR','None',#24191,#830);
#725=SHAPE_REPRESENTATION_RELATIONSHIP('SRR','None',#24192,#831);
#726=SHAPE_REPRESENTATION_RELATIONSHIP('SRR','None',#24193,#832);
#727=SHAPE_REPRESENTATION_RELATIONSHIP('SRR','None',#24195,#833);
#728=SHAPE_REPRESENTATION_RELATIONSHIP('SRR','None',#24196,#834);
#729=SHAPE_REPRESENTATION_RELATIONSHIP('SRR','None',#24197,#835);
#730=SHAPE_REPRESENTATION_RELATIONSHIP('SRR','None',#24198,#836);
#731=SHAPE_REPRESENTATION_RELATIONSHIP('SRR','None',#24199,#837);
#732=SHAPE_REPRESENTATION_RELATIONSHIP('SRR','None',#24200,#838);
#733=SHAPE_REPRESENTATION_RELATIONSHIP('SRR','None',#24201,#839);
#734=SHAPE_REPRESENTATION_RELATIONSHIP('SRR','None',#24202,#840);
#735=SHAPE_REPRESENTATION_RELATIONSHIP('SRR','None',#24203,#841);
#736=SHAPE_REPRESENTATION_RELATIONSHIP('SRR','None',#24204,#842);
#737=SHAPE_REPRESENTATION_RELATIONSHIP('SRR','None',#24205,#843);
#738=SHAPE_REPRESENTATION_RELATIONSHIP('SRR','None',#24206,#844);
#739=SHAPE_REPRESENTATION_RELATIONSHIP('SRR','None',#24207,#845);
#740=SHAPE_REPRESENTATION_RELATIONSHIP('SRR','None',#24209,#846);
#741=SHAPE_REPRESENTATION_RELATIONSHIP('SRR','None',#24210,#847);
#742=SHAPE_REPRESENTATION_RELATIONSHIP('SRR','None',#24211,#848);
#743=SHAPE_REPRESENTATION_RELATIONSHIP('SRR','None',#24212,#849);
#744=SHAPE_REPRESENTATION_RELATIONSHIP('SRR','None',#24213,#850);
#745=SHAPE_REPRESENTATION_RELATIONSHIP('SRR','None',#24214,#851);
#746=SHAPE_REPRESENTATION_RELATIONSHIP('SRR','None',#24215,#852);
#747=SHAPE_REPRESENTATION_RELATIONSHIP('SRR','None',#24217,#853);
#748=SHAPE_REPRESENTATION_RELATIONSHIP('SRR','None',#24218,#854);
#749=SHAPE_REPRESENTATION_RELATIONSHIP('SRR','None',#24219,#855);
#750=SHAPE_REPRESENTATION_RELATIONSHIP('SRR','None',#24221,#856);
#751=SHAPE_REPRESENTATION_RELATIONSHIP('SRR','None',#24223,#857);
#752=SHAPE_REPRESENTATION_RELATIONSHIP('SRR','None',#24224,#858);
#753=SHAPE_REPRESENTATION_RELATIONSHIP('SRR','None',#24225,#859);
#754=SHAPE_REPRESENTATION_RELATIONSHIP('SRR','None',#24226,#860);
#755=SHAPE_REPRESENTATION_RELATIONSHIP('SRR','None',#24227,#861);
#756=ADVANCED_BREP_SHAPE_REPRESENTATION('',(#976),#23614);
#757=ADVANCED_BREP_SHAPE_REPRESENTATION('',(#977),#23615);
#758=ADVANCED_BREP_SHAPE_REPRESENTATION('',(#978),#23616);
#759=ADVANCED_BREP_SHAPE_REPRESENTATION('',(#979),#23617);
#760=ADVANCED_BREP_SHAPE_REPRESENTATION('',(#980),#23618);
#761=ADVANCED_BREP_SHAPE_REPRESENTATION('',(#981),#23619);
#762=ADVANCED_BREP_SHAPE_REPRESENTATION('',(#982),#23620);
#763=ADVANCED_BREP_SHAPE_REPRESENTATION('',(#983),#23621);
#764=ADVANCED_BREP_SHAPE_REPRESENTATION('',(#984),#23622);
#765=ADVANCED_BREP_SHAPE_REPRESENTATION('',(#985),#23623);
#766=ADVANCED_BREP_SHAPE_REPRESENTATION('',(#986),#23624);
#767=ADVANCED_BREP_SHAPE_REPRESENTATION('',(#987),#23625);
#768=ADVANCED_BREP_SHAPE_REPRESENTATION('',(#988),#23626);
#769=ADVANCED_BREP_SHAPE_REPRESENTATION('',(#989),#23627);
#770=ADVANCED_BREP_SHAPE_REPRESENTATION('',(#990),#23628);
#771=ADVANCED_BREP_SHAPE_REPRESENTATION('',(#991),#23629);
#772=ADVANCED_BREP_SHAPE_REPRESENTATION('',(#992),#23630);
#773=ADVANCED_BREP_SHAPE_REPRESENTATION('',(#993),#23631);
#774=ADVANCED_BREP_SHAPE_REPRESENTATION('',(#994),#23632);
#775=ADVANCED_BREP_SHAPE_REPRESENTATION('',(#995),#23633);
#776=ADVANCED_BREP_SHAPE_REPRESENTATION('',(#996),#23634);
#777=ADVANCED_BREP_SHAPE_REPRESENTATION('',(#997),#23635);
#778=ADVANCED_BREP_SHAPE_REPRESENTATION('',(#998),#23636);
#779=ADVANCED_BREP_SHAPE_REPRESENTATION('',(#999),#23637);
#780=ADVANCED_BREP_SHAPE_REPRESENTATION('',(#1000),#23638);
#781=ADVANCED_BREP_SHAPE_REPRESENTATION('',(#1001),#23639);
#782=ADVANCED_BREP_SHAPE_REPRESENTATION('',(#1002),#23640);
#783=ADVANCED_BREP_SHAPE_REPRESENTATION('',(#1003),#23641);
#784=ADVANCED_BREP_SHAPE_REPRESENTATION('',(#1004),#23642);
#785=ADVANCED_BREP_SHAPE_REPRESENTATION('',(#647),#23643);
#786=ADVANCED_BREP_SHAPE_REPRESENTATION('',(#1005),#23645);
#787=ADVANCED_BREP_SHAPE_REPRESENTATION('',(#1006),#23646);
#788=ADVANCED_BREP_SHAPE_REPRESENTATION('',(#1007),#23647);
#789=ADVANCED_BREP_SHAPE_REPRESENTATION('',(#1008),#23648);
#790=ADVANCED_BREP_SHAPE_REPRESENTATION('',(#1009),#23649);
#791=ADVANCED_BREP_SHAPE_REPRESENTATION('',(#1010),#23650);
#792=ADVANCED_BREP_SHAPE_REPRESENTATION('',(#1011),#23651);
#793=ADVANCED_BREP_SHAPE_REPRESENTATION('',(#1012),#23652);
#794=ADVANCED_BREP_SHAPE_REPRESENTATION('',(#1013),#23653);
#795=ADVANCED_BREP_SHAPE_REPRESENTATION('',(#1014),#23654);
#796=ADVANCED_BREP_SHAPE_REPRESENTATION('',(#1015),#23655);
#797=ADVANCED_BREP_SHAPE_REPRESENTATION('',(#1016),#23656);
#798=ADVANCED_BREP_SHAPE_REPRESENTATION('',(#1017),#23657);
#799=ADVANCED_BREP_SHAPE_REPRESENTATION('',(#1018),#23658);
#800=ADVANCED_BREP_SHAPE_REPRESENTATION('',(#1019),#23659);
#801=ADVANCED_BREP_SHAPE_REPRESENTATION('',(#1020),#23660);
#802=ADVANCED_BREP_SHAPE_REPRESENTATION('',(#1021),#23661);
#803=ADVANCED_BREP_SHAPE_REPRESENTATION('',(#1022),#23662);
#804=ADVANCED_BREP_SHAPE_REPRESENTATION('',(#1023),#23663);
#805=ADVANCED_BREP_SHAPE_REPRESENTATION('',(#1024),#23664);
#806=ADVANCED_BREP_SHAPE_REPRESENTATION('',(#1025),#23665);
#807=ADVANCED_BREP_SHAPE_REPRESENTATION('',(#1026),#23667);
#808=ADVANCED_BREP_SHAPE_REPRESENTATION('',(#1027),#23668);
#809=ADVANCED_BREP_SHAPE_REPRESENTATION('',(#1028),#23669);
#810=ADVANCED_BREP_SHAPE_REPRESENTATION('',(#1029),#23670);
#811=ADVANCED_BREP_SHAPE_REPRESENTATION('',(#1030),#23671);
#812=ADVANCED_BREP_SHAPE_REPRESENTATION('',(#1031),#23672);
#813=ADVANCED_BREP_SHAPE_REPRESENTATION('',(#1032),#23673);
#814=ADVANCED_BREP_SHAPE_REPRESENTATION('',(#1033),#23674);
#815=ADVANCED_BREP_SHAPE_REPRESENTATION('',(#1034),#23675);
#816=ADVANCED_BREP_SHAPE_REPRESENTATION('',(#1035),#23676);
#817=ADVANCED_BREP_SHAPE_REPRESENTATION('',(#1036),#23677);
#818=ADVANCED_BREP_SHAPE_REPRESENTATION('',(#1037),#23678);
#819=ADVANCED_BREP_SHAPE_REPRESENTATION('',(#1038),#23679);
#820=ADVANCED_BREP_SHAPE_REPRESENTATION('',(#1039),#23680);
#821=ADVANCED_BREP_SHAPE_REPRESENTATION('',(#1040),#23681);
#822=ADVANCED_BREP_SHAPE_REPRESENTATION('',(#1041),#23682);
#823=ADVANCED_BREP_SHAPE_REPRESENTATION('',(#1042),#23683);
#824=ADVANCED_BREP_SHAPE_REPRESENTATION('',(#1043),#23684);
#825=ADVANCED_BREP_SHAPE_REPRESENTATION('',(#1044),#23685);
#826=ADVANCED_BREP_SHAPE_REPRESENTATION('',(#1045),#23686);
#827=ADVANCED_BREP_SHAPE_REPRESENTATION('',(#1046),#23687);
#828=ADVANCED_BREP_SHAPE_REPRESENTATION('',(#1047),#23689);
#829=ADVANCED_BREP_SHAPE_REPRESENTATION('',(#1048),#23690);
#830=ADVANCED_BREP_SHAPE_REPRESENTATION('',(#1049,#1050,#1051,#1052,#1053,
#1054,#1055),#23691);
#831=ADVANCED_BREP_SHAPE_REPRESENTATION('',(#1056),#23692);
#832=ADVANCED_BREP_SHAPE_REPRESENTATION('',(#1057,#1058),#23693);
#833=ADVANCED_BREP_SHAPE_REPRESENTATION('',(#1059,#1060),#23695);
#834=ADVANCED_BREP_SHAPE_REPRESENTATION('',(#1061),#23696);
#835=ADVANCED_BREP_SHAPE_REPRESENTATION('',(#1062),#23697);
#836=ADVANCED_BREP_SHAPE_REPRESENTATION('',(#1063),#23698);
#837=ADVANCED_BREP_SHAPE_REPRESENTATION('',(#1064),#23699);
#838=ADVANCED_BREP_SHAPE_REPRESENTATION('',(#1065),#23700);
#839=ADVANCED_BREP_SHAPE_REPRESENTATION('',(#1066),#23701);
#840=ADVANCED_BREP_SHAPE_REPRESENTATION('',(#1067),#23702);
#841=ADVANCED_BREP_SHAPE_REPRESENTATION('',(#1068),#23703);
#842=ADVANCED_BREP_SHAPE_REPRESENTATION('',(#1069),#23704);
#843=ADVANCED_BREP_SHAPE_REPRESENTATION('',(#1070),#23705);
#844=ADVANCED_BREP_SHAPE_REPRESENTATION('',(#1071),#23706);
#845=ADVANCED_BREP_SHAPE_REPRESENTATION('',(#648),#23707);
#846=ADVANCED_BREP_SHAPE_REPRESENTATION('',(#1072),#23709);
#847=ADVANCED_BREP_SHAPE_REPRESENTATION('',(#1073),#23710);
#848=ADVANCED_BREP_SHAPE_REPRESENTATION('',(#1074),#23711);
#849=ADVANCED_BREP_SHAPE_REPRESENTATION('',(#1075),#23712);
#850=ADVANCED_BREP_SHAPE_REPRESENTATION('',(#1076),#23713);
#851=ADVANCED_BREP_SHAPE_REPRESENTATION('',(#1077),#23714);
#852=ADVANCED_BREP_SHAPE_REPRESENTATION('',(#1078),#23715);
#853=ADVANCED_BREP_SHAPE_REPRESENTATION('',(#1079),#23717);
#854=ADVANCED_BREP_SHAPE_REPRESENTATION('',(#1080),#23718);
#855=ADVANCED_BREP_SHAPE_REPRESENTATION('',(#649),#23719);
#856=ADVANCED_BREP_SHAPE_REPRESENTATION('',(#1081),#23721);
#857=ADVANCED_BREP_SHAPE_REPRESENTATION('',(#1082),#23723);
#858=ADVANCED_BREP_SHAPE_REPRESENTATION('',(#1083),#23724);
#859=ADVANCED_BREP_SHAPE_REPRESENTATION('',(#1084),#23725);
#860=ADVANCED_BREP_SHAPE_REPRESENTATION('',(#1085),#23726);
#861=ADVANCED_BREP_SHAPE_REPRESENTATION('',(#1086),#23727);
#862=STYLED_ITEM('',(#24744),#976);
#863=STYLED_ITEM('',(#24779),#977);
#864=STYLED_ITEM('',(#24779),#978);
#865=STYLED_ITEM('',(#24779),#979);
#866=STYLED_ITEM('',(#24779),#980);
#867=STYLED_ITEM('',(#24765),#981);
#868=STYLED_ITEM('',(#24758),#982);
#869=STYLED_ITEM('',(#24779),#983);
#870=STYLED_ITEM('',(#24779),#984);
#871=STYLED_ITEM('',(#24765),#985);
#872=STYLED_ITEM('',(#24758),#986);
#873=STYLED_ITEM('',(#24779),#987);
#874=STYLED_ITEM('',(#24779),#988);
#875=STYLED_ITEM('',(#24772),#989);
#876=STYLED_ITEM('',(#24772),#990);
#877=STYLED_ITEM('',(#24772),#991);
#878=STYLED_ITEM('',(#24772),#992);
#879=STYLED_ITEM('',(#24772),#993);
#880=STYLED_ITEM('',(#24772),#994);
#881=STYLED_ITEM('',(#24772),#995);
#882=STYLED_ITEM('',(#24772),#996);
#883=STYLED_ITEM('',(#24772),#997);
#884=STYLED_ITEM('',(#24772),#998);
#885=STYLED_ITEM('',(#24772),#999);
#886=STYLED_ITEM('',(#24772),#1000);
#887=STYLED_ITEM('',(#24772),#1001);
#888=STYLED_ITEM('',(#24772),#1002);
#889=STYLED_ITEM('',(#24765),#1003);
#890=STYLED_ITEM('',(#24765),#1004);
#891=STYLED_ITEM('',(#24772),#647);
#892=STYLED_ITEM('',(#24779),#1005);
#893=STYLED_ITEM('',(#24765),#1006);
#894=STYLED_ITEM('',(#24772),#1007);
#895=STYLED_ITEM('',(#24772),#1008);
#896=STYLED_ITEM('',(#24772),#1009);
#897=STYLED_ITEM('',(#24772),#1010);
#898=STYLED_ITEM('',(#24765),#1011);
#899=STYLED_ITEM('',(#24772),#1012);
#900=STYLED_ITEM('',(#24772),#1013);
#901=STYLED_ITEM('',(#24772),#1014);
#902=STYLED_ITEM('',(#24772),#1015);
#903=STYLED_ITEM('',(#24765),#1016);
#904=STYLED_ITEM('',(#24772),#1017);
#905=STYLED_ITEM('',(#24772),#1018);
#906=STYLED_ITEM('',(#24772),#1019);
#907=STYLED_ITEM('',(#24772),#1020);
#908=STYLED_ITEM('',(#24765),#1021);
#909=STYLED_ITEM('',(#24772),#1022);
#910=STYLED_ITEM('',(#24772),#1023);
#911=STYLED_ITEM('',(#24772),#1024);
#912=STYLED_ITEM('',(#24772),#1025);
#913=STYLED_ITEM('',(#24779),#1026);
#914=STYLED_ITEM('',(#24765),#1027);
#915=STYLED_ITEM('',(#24772),#1028);
#916=STYLED_ITEM('',(#24772),#1029);
#917=STYLED_ITEM('',(#24772),#1030);
#918=STYLED_ITEM('',(#24772),#1031);
#919=STYLED_ITEM('',(#24765),#1032);
#920=STYLED_ITEM('',(#24772),#1033);
#921=STYLED_ITEM('',(#24772),#1034);
#922=STYLED_ITEM('',(#24772),#1035);
#923=STYLED_ITEM('',(#24772),#1036);
#924=STYLED_ITEM('',(#24765),#1037);
#925=STYLED_ITEM('',(#24772),#1038);
#926=STYLED_ITEM('',(#24772),#1039);
#927=STYLED_ITEM('',(#24772),#1040);
#928=STYLED_ITEM('',(#24772),#1041);
#929=STYLED_ITEM('',(#24765),#1042);
#930=STYLED_ITEM('',(#24772),#1043);
#931=STYLED_ITEM('',(#24772),#1044);
#932=STYLED_ITEM('',(#24772),#1045);
#933=STYLED_ITEM('',(#24772),#1046);
#934=STYLED_ITEM('',(#24765),#1047);
#935=STYLED_ITEM('',(#24765),#1048);
#936=STYLED_ITEM('',(#24765),#1049);
#937=STYLED_ITEM('',(#24765),#1050);
#938=STYLED_ITEM('',(#24765),#1051);
#939=STYLED_ITEM('',(#24765),#1052);
#940=STYLED_ITEM('',(#24765),#1053);
#941=STYLED_ITEM('',(#24765),#1054);
#942=STYLED_ITEM('',(#24765),#1055);
#943=STYLED_ITEM('',(#24765),#1056);
#944=STYLED_ITEM('',(#24765),#1057);
#945=STYLED_ITEM('',(#24765),#1058);
#946=STYLED_ITEM('',(#24744),#1059);
#947=STYLED_ITEM('',(#24744),#1060);
#948=STYLED_ITEM('',(#24758),#1061);
#949=STYLED_ITEM('',(#24758),#1062);
#950=STYLED_ITEM('',(#24765),#1063);
#951=STYLED_ITEM('',(#24779),#1064);
#952=STYLED_ITEM('',(#24758),#1065);
#953=STYLED_ITEM('',(#24779),#1066);
#954=STYLED_ITEM('',(#24779),#1067);
#955=STYLED_ITEM('',(#24765),#1068);
#956=STYLED_ITEM('',(#24779),#1069);
#957=STYLED_ITEM('',(#24779),#1070);
#958=STYLED_ITEM('',(#24779),#1071);
#959=STYLED_ITEM('',(#24772),#648);
#960=STYLED_ITEM('',(#24772),#1072);
#961=STYLED_ITEM('',(#24765),#1073);
#962=STYLED_ITEM('',(#24765),#1074);
#963=STYLED_ITEM('',(#24751),#1075);
#964=STYLED_ITEM('',(#24765),#1076);
#965=STYLED_ITEM('',(#24765),#1077);
#966=STYLED_ITEM('',(#24765),#1078);
#967=STYLED_ITEM('',(#24779),#1079);
#968=STYLED_ITEM('',(#24758),#1080);
#969=STYLED_ITEM('',(#24772),#649);
#970=STYLED_ITEM('',(#24758),#1081);
#971=STYLED_ITEM('',(#24772),#1082);
#972=STYLED_ITEM('',(#24772),#1083);
#973=STYLED_ITEM('',(#24772),#1084);
#974=STYLED_ITEM('',(#24758),#1085);
#975=STYLED_ITEM('',(#24772),#1086);
#976=MANIFOLD_SOLID_BREP('Body1',#12392);
#977=MANIFOLD_SOLID_BREP('Body1',#12393);
#978=MANIFOLD_SOLID_BREP('Body1',#12394);
#979=MANIFOLD_SOLID_BREP('Body1',#12395);
#980=MANIFOLD_SOLID_BREP('Body1',#12396);
#981=MANIFOLD_SOLID_BREP('Body1',#12397);
#982=MANIFOLD_SOLID_BREP('Body1',#12398);
#983=MANIFOLD_SOLID_BREP('Body1',#12399);
#984=MANIFOLD_SOLID_BREP('Body1',#12400);
#985=MANIFOLD_SOLID_BREP('Body1',#12401);
#986=MANIFOLD_SOLID_BREP('Body1',#12402);
#987=MANIFOLD_SOLID_BREP('Body1',#12403);
#988=MANIFOLD_SOLID_BREP('Body1',#12404);
#989=MANIFOLD_SOLID_BREP('Body1',#12405);
#990=MANIFOLD_SOLID_BREP('Body1',#12406);
#991=MANIFOLD_SOLID_BREP('Body1',#12407);
#992=MANIFOLD_SOLID_BREP('Body1',#12408);
#993=MANIFOLD_SOLID_BREP('Body1',#12409);
#994=MANIFOLD_SOLID_BREP('Body1',#12410);
#995=MANIFOLD_SOLID_BREP('Body1',#12411);
#996=MANIFOLD_SOLID_BREP('Body1',#12412);
#997=MANIFOLD_SOLID_BREP('Body1',#12413);
#998=MANIFOLD_SOLID_BREP('Body1',#12414);
#999=MANIFOLD_SOLID_BREP('Body1',#12415);
#1000=MANIFOLD_SOLID_BREP('Body1',#12416);
#1001=MANIFOLD_SOLID_BREP('Body1',#12417);
#1002=MANIFOLD_SOLID_BREP('Body1',#12418);
#1003=MANIFOLD_SOLID_BREP('Body1',#12419);
#1004=MANIFOLD_SOLID_BREP('Body1',#12420);
#1005=MANIFOLD_SOLID_BREP('Body1',#12423);
#1006=MANIFOLD_SOLID_BREP('Body1',#12424);
#1007=MANIFOLD_SOLID_BREP('Body1',#12425);
#1008=MANIFOLD_SOLID_BREP('Body1',#12426);
#1009=MANIFOLD_SOLID_BREP('Body1',#12427);
#1010=MANIFOLD_SOLID_BREP('Body1',#12428);
#1011=MANIFOLD_SOLID_BREP('Body1',#12429);
#1012=MANIFOLD_SOLID_BREP('Body1',#12430);
#1013=MANIFOLD_SOLID_BREP('Body1',#12431);
#1014=MANIFOLD_SOLID_BREP('Body1',#12432);
#1015=MANIFOLD_SOLID_BREP('Body1',#12433);
#1016=MANIFOLD_SOLID_BREP('Body1',#12434);
#1017=MANIFOLD_SOLID_BREP('Body1',#12435);
#1018=MANIFOLD_SOLID_BREP('Body1',#12436);
#1019=MANIFOLD_SOLID_BREP('Body1',#12437);
#1020=MANIFOLD_SOLID_BREP('Body1',#12438);
#1021=MANIFOLD_SOLID_BREP('Body1',#12439);
#1022=MANIFOLD_SOLID_BREP('Body1',#12440);
#1023=MANIFOLD_SOLID_BREP('Body1',#12441);
#1024=MANIFOLD_SOLID_BREP('Body1',#12442);
#1025=MANIFOLD_SOLID_BREP('Body1',#12443);
#1026=MANIFOLD_SOLID_BREP('Body1',#12444);
#1027=MANIFOLD_SOLID_BREP('Body1',#12445);
#1028=MANIFOLD_SOLID_BREP('Body1',#12446);
#1029=MANIFOLD_SOLID_BREP('Body1',#12447);
#1030=MANIFOLD_SOLID_BREP('Body1',#12448);
#1031=MANIFOLD_SOLID_BREP('Body1',#12449);
#1032=MANIFOLD_SOLID_BREP('Body1',#12450);
#1033=MANIFOLD_SOLID_BREP('Body1',#12451);
#1034=MANIFOLD_SOLID_BREP('Body1',#12452);
#1035=MANIFOLD_SOLID_BREP('Body1',#12453);
#1036=MANIFOLD_SOLID_BREP('Body1',#12454);
#1037=MANIFOLD_SOLID_BREP('Body1',#12455);
#1038=MANIFOLD_SOLID_BREP('Body1',#12456);
#1039=MANIFOLD_SOLID_BREP('Body1',#12457);
#1040=MANIFOLD_SOLID_BREP('Body1',#12458);
#1041=MANIFOLD_SOLID_BREP('Body1',#12459);
#1042=MANIFOLD_SOLID_BREP('Body1',#12460);
#1043=MANIFOLD_SOLID_BREP('Body1',#12461);
#1044=MANIFOLD_SOLID_BREP('Body1',#12462);
#1045=MANIFOLD_SOLID_BREP('Body1',#12463);
#1046=MANIFOLD_SOLID_BREP('Body1',#12464);
#1047=MANIFOLD_SOLID_BREP('Body1',#12465);
#1048=MANIFOLD_SOLID_BREP('Body1',#12466);
#1049=MANIFOLD_SOLID_BREP('Body1',#12467);
#1050=MANIFOLD_SOLID_BREP('Body2',#12468);
#1051=MANIFOLD_SOLID_BREP('Body3',#12469);
#1052=MANIFOLD_SOLID_BREP('Body4',#12470);
#1053=MANIFOLD_SOLID_BREP('Body5',#12471);
#1054=MANIFOLD_SOLID_BREP('Body6',#12472);
#1055=MANIFOLD_SOLID_BREP('Body7',#12473);
#1056=MANIFOLD_SOLID_BREP('Continuous crown cage',#12474);
#1057=MANIFOLD_SOLID_BREP('Body1',#12475);
#1058=MANIFOLD_SOLID_BREP('Body2',#12476);
#1059=MANIFOLD_SOLID_BREP('Body1',#12477);
#1060=MANIFOLD_SOLID_BREP('Body2',#12478);
#1061=MANIFOLD_SOLID_BREP('Body1',#12479);
#1062=MANIFOLD_SOLID_BREP('Body1',#12480);
#1063=MANIFOLD_SOLID_BREP('Body1',#12481);
#1064=MANIFOLD_SOLID_BREP('Body1',#12482);
#1065=MANIFOLD_SOLID_BREP('Body1',#12483);
#1066=MANIFOLD_SOLID_BREP('Body1',#12484);
#1067=MANIFOLD_SOLID_BREP('Body1',#12485);
#1068=MANIFOLD_SOLID_BREP('Body1',#12486);
#1069=MANIFOLD_SOLID_BREP('Body1',#12487);
#1070=MANIFOLD_SOLID_BREP('Body1',#12488);
#1071=MANIFOLD_SOLID_BREP('Body1',#12489);
#1072=MANIFOLD_SOLID_BREP('Body1',#12492);
#1073=MANIFOLD_SOLID_BREP('Body1',#12493);
#1074=MANIFOLD_SOLID_BREP('Body1',#12494);
#1075=MANIFOLD_SOLID_BREP('Body1',#12495);
#1076=MANIFOLD_SOLID_BREP('Body1',#12496);
#1077=MANIFOLD_SOLID_BREP('Body1',#12497);
#1078=MANIFOLD_SOLID_BREP('Body1',#12498);
#1079=MANIFOLD_SOLID_BREP('Body1',#12499);
#1080=MANIFOLD_SOLID_BREP('Body1',#12500);
#1081=MANIFOLD_SOLID_BREP('Body1',#12503);
#1082=MANIFOLD_SOLID_BREP('Body1',#12504);
#1083=MANIFOLD_SOLID_BREP('Body1',#12505);
#1084=MANIFOLD_SOLID_BREP('Body1',#12506);
#1085=MANIFOLD_SOLID_BREP('Body1',#12507);
#1086=MANIFOLD_SOLID_BREP('Body1',#12508);
#1087=FACE_BOUND('',#2684,.T.);
#1088=FACE_BOUND('',#2685,.T.);
#1089=FACE_BOUND('',#2686,.T.);
#1090=FACE_BOUND('',#2687,.T.);
#1091=FACE_BOUND('',#2688,.T.);
#1092=FACE_BOUND('',#2689,.T.);
#1093=FACE_BOUND('',#2690,.T.);
#1094=FACE_BOUND('',#2691,.T.);
#1095=FACE_BOUND('',#2692,.T.);
#1096=FACE_BOUND('',#2693,.T.);
#1097=FACE_BOUND('',#2694,.T.);
#1098=FACE_BOUND('',#2695,.T.);
#1099=FACE_BOUND('',#2697,.T.);
#1100=FACE_BOUND('',#2698,.T.);
#1101=FACE_BOUND('',#2699,.T.);
#1102=FACE_BOUND('',#2700,.T.);
#1103=FACE_BOUND('',#2701,.T.);
#1104=FACE_BOUND('',#2702,.T.);
#1105=FACE_BOUND('',#2703,.T.);
#1106=FACE_BOUND('',#2704,.T.);
#1107=FACE_BOUND('',#2705,.T.);
#1108=FACE_BOUND('',#2706,.T.);
#1109=FACE_BOUND('',#2707,.T.);
#1110=FACE_BOUND('',#2708,.T.);
#1111=FACE_BOUND('',#2730,.T.);
#1112=FACE_BOUND('',#2731,.T.);
#1113=FACE_BOUND('',#2732,.T.);
#1114=FACE_BOUND('',#2733,.T.);
#1115=FACE_BOUND('',#2738,.T.);
#1116=FACE_BOUND('',#2739,.T.);
#1117=FACE_BOUND('',#2740,.T.);
#1118=FACE_BOUND('',#2741,.T.);
#1119=FACE_BOUND('',#2744,.T.);
#1120=FACE_BOUND('',#2745,.T.);
#1121=FACE_BOUND('',#2746,.T.);
#1122=FACE_BOUND('',#2747,.T.);
#1123=FACE_BOUND('',#2751,.T.);
#1124=FACE_BOUND('',#2752,.T.);
#1125=FACE_BOUND('',#2753,.T.);
#1126=FACE_BOUND('',#2754,.T.);
#1127=FACE_BOUND('',#2764,.T.);
#1128=FACE_BOUND('',#2765,.T.);
#1129=FACE_BOUND('',#2766,.T.);
#1130=FACE_BOUND('',#2767,.T.);
#1131=FACE_BOUND('',#2772,.T.);
#1132=FACE_BOUND('',#2773,.T.);
#1133=FACE_BOUND('',#2774,.T.);
#1134=FACE_BOUND('',#2775,.T.);
#1135=FACE_BOUND('',#2778,.T.);
#1136=FACE_BOUND('',#2779,.T.);
#1137=FACE_BOUND('',#2780,.T.);
#1138=FACE_BOUND('',#2781,.T.);
#1139=FACE_BOUND('',#2785,.T.);
#1140=FACE_BOUND('',#2786,.T.);
#1141=FACE_BOUND('',#2787,.T.);
#1142=FACE_BOUND('',#2788,.T.);
#1143=FACE_BOUND('',#2795,.T.);
#1144=FACE_BOUND('',#2796,.T.);
#1145=FACE_BOUND('',#2797,.T.);
#1146=FACE_BOUND('',#2798,.T.);
#1147=FACE_BOUND('',#2800,.T.);
#1148=FACE_BOUND('',#2801,.T.);
#1149=FACE_BOUND('',#2802,.T.);
#1150=FACE_BOUND('',#2803,.T.);
#1151=FACE_BOUND('',#2809,.T.);
#1152=FACE_BOUND('',#2813,.T.);
#1153=FACE_BOUND('',#2815,.T.);
#1154=FACE_BOUND('',#2819,.T.);
#1155=FACE_BOUND('',#2821,.T.);
#1156=FACE_BOUND('',#2825,.T.);
#1157=FACE_BOUND('',#2827,.T.);
#1158=FACE_BOUND('',#2834,.T.);
#1159=FACE_BOUND('',#2835,.T.);
#1160=FACE_BOUND('',#2836,.T.);
#1161=FACE_BOUND('',#2837,.T.);
#1162=FACE_BOUND('',#2839,.T.);
#1163=FACE_BOUND('',#2840,.T.);
#1164=FACE_BOUND('',#2841,.T.);
#1165=FACE_BOUND('',#2842,.T.);
#1166=FACE_BOUND('',#2848,.T.);
#1167=FACE_BOUND('',#2852,.T.);
#1168=FACE_BOUND('',#2854,.T.);
#1169=FACE_BOUND('',#2858,.T.);
#1170=FACE_BOUND('',#2860,.T.);
#1171=FACE_BOUND('',#2864,.T.);
#1172=FACE_BOUND('',#2866,.T.);
#1173=FACE_BOUND('',#2870,.T.);
#1174=FACE_BOUND('',#2872,.T.);
#1175=FACE_BOUND('',#2873,.T.);
#1176=FACE_BOUND('',#2874,.T.);
#1177=FACE_BOUND('',#2875,.T.);
#1178=FACE_BOUND('',#2878,.T.);
#1179=FACE_BOUND('',#2882,.T.);
#1180=FACE_BOUND('',#2890,.T.);
#1181=FACE_BOUND('',#2891,.T.);
#1182=FACE_BOUND('',#2892,.T.);
#1183=FACE_BOUND('',#2893,.T.);
#1184=FACE_BOUND('',#2895,.T.);
#1185=FACE_BOUND('',#2897,.T.);
#1186=FACE_BOUND('',#2898,.T.);
#1187=FACE_BOUND('',#2904,.T.);
#1188=FACE_BOUND('',#2905,.T.);
#1189=FACE_BOUND('',#2906,.T.);
#1190=FACE_BOUND('',#2911,.T.);
#1191=FACE_BOUND('',#2912,.T.);
#1192=FACE_BOUND('',#2913,.T.);
#1193=FACE_BOUND('',#2915,.T.);
#1194=FACE_BOUND('',#2921,.T.);
#1195=FACE_BOUND('',#2931,.T.);
#1196=FACE_BOUND('',#2932,.T.);
#1197=FACE_BOUND('',#2933,.T.);
#1198=FACE_BOUND('',#2938,.T.);
#1199=FACE_BOUND('',#2939,.T.);
#1200=FACE_BOUND('',#2940,.T.);
#1201=FACE_BOUND('',#2942,.T.);
#1202=FACE_BOUND('',#2948,.T.);
#1203=FACE_BOUND('',#2956,.T.);
#1204=FACE_BOUND('',#2958,.T.);
#1205=FACE_BOUND('',#2959,.T.);
#1206=FACE_BOUND('',#2960,.T.);
#1207=FACE_BOUND('',#2961,.T.);
#1208=FACE_BOUND('',#2964,.T.);
#1209=FACE_BOUND('',#2968,.T.);
#1210=FACE_BOUND('',#2976,.T.);
#1211=FACE_BOUND('',#2977,.T.);
#1212=FACE_BOUND('',#2978,.T.);
#1213=FACE_BOUND('',#2979,.T.);
#1214=FACE_BOUND('',#2981,.T.);
#1215=FACE_BOUND('',#2983,.T.);
#1216=FACE_BOUND('',#2984,.T.);
#1217=FACE_BOUND('',#2990,.T.);
#1218=FACE_BOUND('',#2991,.T.);
#1219=FACE_BOUND('',#2992,.T.);
#1220=FACE_BOUND('',#2997,.T.);
#1221=FACE_BOUND('',#2998,.T.);
#1222=FACE_BOUND('',#2999,.T.);
#1223=FACE_BOUND('',#3001,.T.);
#1224=FACE_BOUND('',#3007,.T.);
#1225=FACE_BOUND('',#3017,.T.);
#1226=FACE_BOUND('',#3018,.T.);
#1227=FACE_BOUND('',#3019,.T.);
#1228=FACE_BOUND('',#3024,.T.);
#1229=FACE_BOUND('',#3025,.T.);
#1230=FACE_BOUND('',#3026,.T.);
#1231=FACE_BOUND('',#3028,.T.);
#1232=FACE_BOUND('',#3034,.T.);
#1233=FACE_BOUND('',#3050,.T.);
#1234=FACE_BOUND('',#3070,.T.);
#1235=FACE_BOUND('',#3071,.T.);
#1236=FACE_BOUND('',#3072,.T.);
#1237=FACE_BOUND('',#3073,.T.);
#1238=FACE_BOUND('',#3074,.T.);
#1239=FACE_BOUND('',#3075,.T.);
#1240=FACE_BOUND('',#3076,.T.);
#1241=FACE_BOUND('',#3077,.T.);
#1242=FACE_BOUND('',#3078,.T.);
#1243=FACE_BOUND('',#3079,.T.);
#1244=FACE_BOUND('',#3089,.T.);
#1245=FACE_BOUND('',#3090,.T.);
#1246=FACE_BOUND('',#3091,.T.);
#1247=FACE_BOUND('',#3092,.T.);
#1248=FACE_BOUND('',#3093,.T.);
#1249=FACE_BOUND('',#3094,.T.);
#1250=FACE_BOUND('',#3095,.T.);
#1251=FACE_BOUND('',#3096,.T.);
#1252=FACE_BOUND('',#3097,.T.);
#1253=FACE_BOUND('',#3098,.T.);
#1254=FACE_BOUND('',#3106,.T.);
#1255=FACE_BOUND('',#3107,.T.);
#1256=FACE_BOUND('',#3108,.T.);
#1257=FACE_BOUND('',#3109,.T.);
#1258=FACE_BOUND('',#3110,.T.);
#1259=FACE_BOUND('',#3112,.T.);
#1260=FACE_BOUND('',#3113,.T.);
#1261=FACE_BOUND('',#3114,.T.);
#1262=FACE_BOUND('',#3115,.T.);
#1263=FACE_BOUND('',#3116,.T.);
#1264=FACE_BOUND('',#3118,.T.);
#1265=FACE_BOUND('',#3124,.T.);
#1266=FACE_BOUND('',#3130,.T.);
#1267=FACE_BOUND('',#3136,.T.);
#1268=FACE_BOUND('',#3148,.T.);
#1269=FACE_BOUND('',#3149,.T.);
#1270=FACE_BOUND('',#3150,.T.);
#1271=FACE_BOUND('',#3151,.T.);
#1272=FACE_BOUND('',#3152,.T.);
#1273=FACE_BOUND('',#3154,.T.);
#1274=FACE_BOUND('',#3155,.T.);
#1275=FACE_BOUND('',#3156,.T.);
#1276=FACE_BOUND('',#3157,.T.);
#1277=FACE_BOUND('',#3158,.T.);
#1278=FACE_BOUND('',#3160,.T.);
#1279=FACE_BOUND('',#3166,.T.);
#1280=FACE_BOUND('',#3172,.T.);
#1281=FACE_BOUND('',#3178,.T.);
#1282=FACE_BOUND('',#3190,.T.);
#1283=FACE_BOUND('',#3191,.T.);
#1284=FACE_BOUND('',#3192,.T.);
#1285=FACE_BOUND('',#3193,.T.);
#1286=FACE_BOUND('',#3194,.T.);
#1287=FACE_BOUND('',#3196,.T.);
#1288=FACE_BOUND('',#3197,.T.);
#1289=FACE_BOUND('',#3198,.T.);
#1290=FACE_BOUND('',#3199,.T.);
#1291=FACE_BOUND('',#3200,.T.);
#1292=FACE_BOUND('',#3202,.T.);
#1293=FACE_BOUND('',#3208,.T.);
#1294=FACE_BOUND('',#3214,.T.);
#1295=FACE_BOUND('',#3220,.T.);
#1296=FACE_BOUND('',#3232,.T.);
#1297=FACE_BOUND('',#3233,.T.);
#1298=FACE_BOUND('',#3234,.T.);
#1299=FACE_BOUND('',#3235,.T.);
#1300=FACE_BOUND('',#3236,.T.);
#1301=FACE_BOUND('',#3238,.T.);
#1302=FACE_BOUND('',#3239,.T.);
#1303=FACE_BOUND('',#3240,.T.);
#1304=FACE_BOUND('',#3241,.T.);
#1305=FACE_BOUND('',#3242,.T.);
#1306=FACE_BOUND('',#3244,.T.);
#1307=FACE_BOUND('',#3250,.T.);
#1308=FACE_BOUND('',#3256,.T.);
#1309=FACE_BOUND('',#3262,.T.);
#1310=FACE_BOUND('',#3275,.T.);
#1311=FACE_BOUND('',#3276,.T.);
#1312=FACE_BOUND('',#3277,.T.);
#1313=FACE_BOUND('',#3278,.T.);
#1314=FACE_BOUND('',#3279,.T.);
#1315=FACE_BOUND('',#3280,.T.);
#1316=FACE_BOUND('',#3281,.T.);
#1317=FACE_BOUND('',#3282,.T.);
#1318=FACE_BOUND('',#3283,.T.);
#1319=FACE_BOUND('',#3284,.T.);
#1320=FACE_BOUND('',#3293,.T.);
#1321=FACE_BOUND('',#3294,.T.);
#1322=FACE_BOUND('',#3295,.T.);
#1323=FACE_BOUND('',#3296,.T.);
#1324=FACE_BOUND('',#3297,.T.);
#1325=FACE_BOUND('',#3298,.T.);
#1326=FACE_BOUND('',#3299,.T.);
#1327=FACE_BOUND('',#3300,.T.);
#1328=FACE_BOUND('',#3301,.T.);
#1329=FACE_BOUND('',#3302,.T.);
#1330=FACE_BOUND('',#3310,.T.);
#1331=FACE_BOUND('',#3311,.T.);
#1332=FACE_BOUND('',#3312,.T.);
#1333=FACE_BOUND('',#3313,.T.);
#1334=FACE_BOUND('',#3314,.T.);
#1335=FACE_BOUND('',#3316,.T.);
#1336=FACE_BOUND('',#3317,.T.);
#1337=FACE_BOUND('',#3318,.T.);
#1338=FACE_BOUND('',#3319,.T.);
#1339=FACE_BOUND('',#3320,.T.);
#1340=FACE_BOUND('',#3322,.T.);
#1341=FACE_BOUND('',#3328,.T.);
#1342=FACE_BOUND('',#3334,.T.);
#1343=FACE_BOUND('',#3340,.T.);
#1344=FACE_BOUND('',#3352,.T.);
#1345=FACE_BOUND('',#3353,.T.);
#1346=FACE_BOUND('',#3354,.T.);
#1347=FACE_BOUND('',#3355,.T.);
#1348=FACE_BOUND('',#3356,.T.);
#1349=FACE_BOUND('',#3358,.T.);
#1350=FACE_BOUND('',#3359,.T.);
#1351=FACE_BOUND('',#3360,.T.);
#1352=FACE_BOUND('',#3361,.T.);
#1353=FACE_BOUND('',#3362,.T.);
#1354=FACE_BOUND('',#3364,.T.);
#1355=FACE_BOUND('',#3370,.T.);
#1356=FACE_BOUND('',#3376,.T.);
#1357=FACE_BOUND('',#3382,.T.);
#1358=FACE_BOUND('',#3394,.T.);
#1359=FACE_BOUND('',#3395,.T.);
#1360=FACE_BOUND('',#3396,.T.);
#1361=FACE_BOUND('',#3397,.T.);
#1362=FACE_BOUND('',#3398,.T.);
#1363=FACE_BOUND('',#3400,.T.);
#1364=FACE_BOUND('',#3401,.T.);
#1365=FACE_BOUND('',#3402,.T.);
#1366=FACE_BOUND('',#3403,.T.);
#1367=FACE_BOUND('',#3404,.T.);
#1368=FACE_BOUND('',#3406,.T.);
#1369=FACE_BOUND('',#3412,.T.);
#1370=FACE_BOUND('',#3418,.T.);
#1371=FACE_BOUND('',#3424,.T.);
#1372=FACE_BOUND('',#3436,.T.);
#1373=FACE_BOUND('',#3437,.T.);
#1374=FACE_BOUND('',#3438,.T.);
#1375=FACE_BOUND('',#3439,.T.);
#1376=FACE_BOUND('',#3440,.T.);
#1377=FACE_BOUND('',#3442,.T.);
#1378=FACE_BOUND('',#3443,.T.);
#1379=FACE_BOUND('',#3444,.T.);
#1380=FACE_BOUND('',#3445,.T.);
#1381=FACE_BOUND('',#3446,.T.);
#1382=FACE_BOUND('',#3448,.T.);
#1383=FACE_BOUND('',#3454,.T.);
#1384=FACE_BOUND('',#3460,.T.);
#1385=FACE_BOUND('',#3466,.T.);
#1386=FACE_BOUND('',#3476,.T.);
#1387=FACE_BOUND('',#3479,.T.);
#1388=FACE_BOUND('',#3484,.T.);
#1389=FACE_BOUND('',#3489,.T.);
#1390=FACE_BOUND('',#3514,.T.);
#1391=FACE_BOUND('',#3517,.T.);
#1392=FACE_BOUND('',#3520,.T.);
#1393=FACE_BOUND('',#3523,.T.);
#1394=FACE_BOUND('',#3526,.T.);
#1395=FACE_BOUND('',#3542,.T.);
#1396=FACE_BOUND('',#3543,.T.);
#1397=FACE_BOUND('',#3544,.T.);
#1398=FACE_BOUND('',#3545,.T.);
#1399=FACE_BOUND('',#3546,.T.);
#1400=FACE_BOUND('',#3547,.T.);
#1401=FACE_BOUND('',#3548,.T.);
#1402=FACE_BOUND('',#3549,.T.);
#1403=FACE_BOUND('',#3557,.T.);
#1404=FACE_BOUND('',#3558,.T.);
#1405=FACE_BOUND('',#3559,.T.);
#1406=FACE_BOUND('',#3560,.T.);
#1407=FACE_BOUND('',#3561,.T.);
#1408=FACE_BOUND('',#3562,.T.);
#1409=FACE_BOUND('',#3563,.T.);
#1410=FACE_BOUND('',#3564,.T.);
#1411=FACE_BOUND('',#3589,.T.);
#1412=FACE_BOUND('',#3590,.T.);
#1413=FACE_BOUND('',#3591,.T.);
#1414=FACE_BOUND('',#3592,.T.);
#1415=FACE_BOUND('',#3594,.T.);
#1416=FACE_BOUND('',#3595,.T.);
#1417=FACE_BOUND('',#3596,.T.);
#1418=FACE_BOUND('',#3597,.T.);
#1419=FACE_BOUND('',#3603,.T.);
#1420=FACE_BOUND('',#3607,.T.);
#1421=FACE_BOUND('',#3609,.T.);
#1422=FACE_BOUND('',#3613,.T.);
#1423=FACE_BOUND('',#3615,.T.);
#1424=FACE_BOUND('',#3619,.T.);
#1425=FACE_BOUND('',#3621,.T.);
#1426=FACE_BOUND('',#3625,.T.);
#1427=FACE_BOUND('',#3627,.T.);
#1428=FACE_BOUND('',#3634,.T.);
#1429=FACE_BOUND('',#3635,.T.);
#1430=FACE_BOUND('',#3636,.T.);
#1431=FACE_BOUND('',#3637,.T.);
#1432=FACE_BOUND('',#3639,.T.);
#1433=FACE_BOUND('',#3640,.T.);
#1434=FACE_BOUND('',#3641,.T.);
#1435=FACE_BOUND('',#3642,.T.);
#1436=FACE_BOUND('',#3648,.T.);
#1437=FACE_BOUND('',#3652,.T.);
#1438=FACE_BOUND('',#3654,.T.);
#1439=FACE_BOUND('',#3658,.T.);
#1440=FACE_BOUND('',#3660,.T.);
#1441=FACE_BOUND('',#3664,.T.);
#1442=FACE_BOUND('',#3666,.T.);
#1443=FACE_BOUND('',#3672,.T.);
#1444=FACE_BOUND('',#3690,.T.);
#1445=FACE_BOUND('',#3691,.T.);
#1446=FACE_BOUND('',#3692,.T.);
#1447=FACE_BOUND('',#3695,.T.);
#1448=FACE_BOUND('',#3696,.T.);
#1449=FACE_BOUND('',#3697,.T.);
#1450=FACE_BOUND('',#3708,.T.);
#1451=FACE_BOUND('',#3709,.T.);
#1452=FACE_BOUND('',#3710,.T.);
#1453=FACE_BOUND('',#3712,.T.);
#1454=FACE_BOUND('',#3713,.T.);
#1455=FACE_BOUND('',#3714,.T.);
#1456=FACE_BOUND('',#3723,.T.);
#1457=FACE_BOUND('',#3724,.T.);
#1458=FACE_BOUND('',#3725,.T.);
#1459=FACE_BOUND('',#3727,.T.);
#1460=FACE_BOUND('',#3728,.T.);
#1461=FACE_BOUND('',#3729,.T.);
#1462=FACE_BOUND('',#3732,.T.);
#1463=FACE_BOUND('',#3735,.T.);
#1464=FACE_BOUND('',#3742,.T.);
#1465=FACE_BOUND('',#3747,.T.);
#1466=FACE_BOUND('',#3751,.T.);
#1467=FACE_BOUND('',#3753,.T.);
#1468=FACE_BOUND('',#3757,.T.);
#1469=FACE_BOUND('',#3759,.T.);
#1470=FACE_BOUND('',#3766,.T.);
#1471=FACE_BOUND('',#3769,.T.);
#1472=FACE_BOUND('',#3772,.T.);
#1473=FACE_BOUND('',#3775,.T.);
#1474=FACE_BOUND('',#3778,.T.);
#1475=FACE_BOUND('',#3781,.T.);
#1476=FACE_BOUND('',#3783,.T.);
#1477=FACE_BOUND('',#3789,.T.);
#1478=FACE_BOUND('',#3791,.T.);
#1479=FACE_BOUND('',#3793,.T.);
#1480=FACE_BOUND('',#3795,.T.);
#1481=FACE_BOUND('',#3810,.T.);
#1482=FACE_BOUND('',#3816,.T.);
#1483=FACE_BOUND('',#3817,.T.);
#1484=FACE_BOUND('',#3823,.T.);
#1485=FACE_BOUND('',#3824,.T.);
#1486=FACE_BOUND('',#3831,.T.);
#1487=FACE_BOUND('',#3833,.T.);
#1488=FACE_BOUND('',#3837,.T.);
#1489=FACE_BOUND('',#3839,.T.);
#1490=FACE_BOUND('',#3843,.T.);
#1491=FACE_BOUND('',#3845,.T.);
#1492=PLANE('',#13715);
#1493=PLANE('',#13716);
#1494=PLANE('',#13717);
#1495=PLANE('',#13718);
#1496=PLANE('',#13719);
#1497=PLANE('',#13720);
#1498=PLANE('',#13722);
#1499=PLANE('',#13723);
#1500=PLANE('',#13724);
#1501=PLANE('',#13725);
#1502=PLANE('',#13726);
#1503=PLANE('',#13727);
#1504=PLANE('',#13729);
#1505=PLANE('',#13730);
#1506=PLANE('',#13731);
#1507=PLANE('',#13732);
#1508=PLANE('',#13733);
#1509=PLANE('',#13734);
#1510=PLANE('',#13760);
#1511=PLANE('',#13761);
#1512=PLANE('',#13762);
#1513=PLANE('',#13763);
#1514=PLANE('',#13764);
#1515=PLANE('',#13765);
#1516=PLANE('',#13766);
#1517=PLANE('',#13767);
#1518=PLANE('',#13768);
#1519=PLANE('',#13769);
#1520=PLANE('',#13795);
#1521=PLANE('',#13796);
#1522=PLANE('',#13797);
#1523=PLANE('',#13798);
#1524=PLANE('',#13799);
#1525=PLANE('',#13800);
#1526=PLANE('',#13801);
#1527=PLANE('',#13802);
#1528=PLANE('',#13803);
#1529=PLANE('',#13804);
#1530=PLANE('',#13809);
#1531=PLANE('',#13819);
#1532=PLANE('',#13822);
#1533=PLANE('',#13830);
#1534=PLANE('',#13831);
#1535=PLANE('',#13839);
#1536=PLANE('',#13840);
#1537=PLANE('',#13848);
#1538=PLANE('',#13849);
#1539=PLANE('',#13857);
#1540=PLANE('',#13858);
#1541=PLANE('',#13863);
#1542=PLANE('',#13873);
#1543=PLANE('',#13876);
#1544=PLANE('',#13884);
#1545=PLANE('',#13885);
#1546=PLANE('',#13893);
#1547=PLANE('',#13894);
#1548=PLANE('',#13902);
#1549=PLANE('',#13903);
#1550=PLANE('',#13911);
#1551=PLANE('',#13912);
#1552=PLANE('',#13920);
#1553=PLANE('',#13922);
#1554=PLANE('',#13929);
#1555=PLANE('',#13935);
#1556=PLANE('',#13945);
#1557=PLANE('',#13946);
#1558=PLANE('',#13947);
#1559=PLANE('',#13948);
#1560=PLANE('',#13949);
#1561=PLANE('',#13963);
#1562=PLANE('',#13973);
#1563=PLANE('',#13975);
#1564=PLANE('',#13980);
#1565=PLANE('',#13983);
#1566=PLANE('',#13985);
#1567=PLANE('',#13990);
#1568=PLANE('',#13993);
#1569=PLANE('',#14007);
#1570=PLANE('',#14017);
#1571=PLANE('',#14019);
#1572=PLANE('',#14024);
#1573=PLANE('',#14027);
#1574=PLANE('',#14029);
#1575=PLANE('',#14034);
#1576=PLANE('',#14037);
#1577=PLANE('',#14045);
#1578=PLANE('',#14047);
#1579=PLANE('',#14054);
#1580=PLANE('',#14060);
#1581=PLANE('',#14070);
#1582=PLANE('',#14071);
#1583=PLANE('',#14072);
#1584=PLANE('',#14073);
#1585=PLANE('',#14074);
#1586=PLANE('',#14088);
#1587=PLANE('',#14098);
#1588=PLANE('',#14100);
#1589=PLANE('',#14105);
#1590=PLANE('',#14108);
#1591=PLANE('',#14110);
#1592=PLANE('',#14115);
#1593=PLANE('',#14118);
#1594=PLANE('',#14132);
#1595=PLANE('',#14142);
#1596=PLANE('',#14144);
#1597=PLANE('',#14149);
#1598=PLANE('',#14152);
#1599=PLANE('',#14154);
#1600=PLANE('',#14159);
#1601=PLANE('',#14162);
#1602=PLANE('',#14167);
#1603=PLANE('',#14168);
#1604=PLANE('',#14173);
#1605=PLANE('',#14174);
#1606=PLANE('',#14176);
#1607=PLANE('',#14184);
#1608=PLANE('',#14192);
#1609=PLANE('',#14193);
#1610=PLANE('',#14194);
#1611=PLANE('',#14195);
#1612=PLANE('',#14196);
#1613=PLANE('',#14197);
#1614=PLANE('',#14198);
#1615=PLANE('',#14199);
#1616=PLANE('',#14200);
#1617=PLANE('',#14221);
#1618=PLANE('',#14228);
#1619=PLANE('',#14241);
#1620=PLANE('',#14242);
#1621=PLANE('',#14262);
#1622=PLANE('',#14263);
#1623=PLANE('',#14265);
#1624=PLANE('',#14270);
#1625=PLANE('',#14273);
#1626=PLANE('',#14275);
#1627=PLANE('',#14280);
#1628=PLANE('',#14283);
#1629=PLANE('',#14285);
#1630=PLANE('',#14290);
#1631=PLANE('',#14293);
#1632=PLANE('',#14295);
#1633=PLANE('',#14300);
#1634=PLANE('',#14303);
#1635=PLANE('',#14323);
#1636=PLANE('',#14324);
#1637=PLANE('',#14326);
#1638=PLANE('',#14331);
#1639=PLANE('',#14334);
#1640=PLANE('',#14336);
#1641=PLANE('',#14341);
#1642=PLANE('',#14344);
#1643=PLANE('',#14346);
#1644=PLANE('',#14351);
#1645=PLANE('',#14354);
#1646=PLANE('',#14356);
#1647=PLANE('',#14361);
#1648=PLANE('',#14364);
#1649=PLANE('',#14384);
#1650=PLANE('',#14385);
#1651=PLANE('',#14387);
#1652=PLANE('',#14392);
#1653=PLANE('',#14395);
#1654=PLANE('',#14397);
#1655=PLANE('',#14402);
#1656=PLANE('',#14405);
#1657=PLANE('',#14407);
#1658=PLANE('',#14412);
#1659=PLANE('',#14415);
#1660=PLANE('',#14417);
#1661=PLANE('',#14422);
#1662=PLANE('',#14425);
#1663=PLANE('',#14445);
#1664=PLANE('',#14446);
#1665=PLANE('',#14448);
#1666=PLANE('',#14453);
#1667=PLANE('',#14456);
#1668=PLANE('',#14458);
#1669=PLANE('',#14463);
#1670=PLANE('',#14466);
#1671=PLANE('',#14468);
#1672=PLANE('',#14473);
#1673=PLANE('',#14476);
#1674=PLANE('',#14478);
#1675=PLANE('',#14483);
#1676=PLANE('',#14486);
#1677=PLANE('',#14507);
#1678=PLANE('',#14508);
#1679=PLANE('',#14527);
#1680=PLANE('',#14528);
#1681=PLANE('',#14548);
#1682=PLANE('',#14549);
#1683=PLANE('',#14551);
#1684=PLANE('',#14556);
#1685=PLANE('',#14559);
#1686=PLANE('',#14561);
#1687=PLANE('',#14566);
#1688=PLANE('',#14569);
#1689=PLANE('',#14571);
#1690=PLANE('',#14576);
#1691=PLANE('',#14579);
#1692=PLANE('',#14581);
#1693=PLANE('',#14586);
#1694=PLANE('',#14589);
#1695=PLANE('',#14609);
#1696=PLANE('',#14610);
#1697=PLANE('',#14612);
#1698=PLANE('',#14617);
#1699=PLANE('',#14620);
#1700=PLANE('',#14622);
#1701=PLANE('',#14627);
#1702=PLANE('',#14630);
#1703=PLANE('',#14632);
#1704=PLANE('',#14637);
#1705=PLANE('',#14640);
#1706=PLANE('',#14642);
#1707=PLANE('',#14647);
#1708=PLANE('',#14650);
#1709=PLANE('',#14670);
#1710=PLANE('',#14671);
#1711=PLANE('',#14673);
#1712=PLANE('',#14678);
#1713=PLANE('',#14681);
#1714=PLANE('',#14683);
#1715=PLANE('',#14688);
#1716=PLANE('',#14691);
#1717=PLANE('',#14693);
#1718=PLANE('',#14698);
#1719=PLANE('',#14701);
#1720=PLANE('',#14703);
#1721=PLANE('',#14708);
#1722=PLANE('',#14711);
#1723=PLANE('',#14731);
#1724=PLANE('',#14732);
#1725=PLANE('',#14734);
#1726=PLANE('',#14739);
#1727=PLANE('',#14742);
#1728=PLANE('',#14744);
#1729=PLANE('',#14749);
#1730=PLANE('',#14752);
#1731=PLANE('',#14754);
#1732=PLANE('',#14759);
#1733=PLANE('',#14762);
#1734=PLANE('',#14764);
#1735=PLANE('',#14769);
#1736=PLANE('',#14772);
#1737=PLANE('',#14788);
#1738=PLANE('',#14791);
#1739=PLANE('',#14803);
#1740=PLANE('',#14812);
#1741=PLANE('',#14843);
#1742=PLANE('',#14848);
#1743=PLANE('',#14853);
#1744=PLANE('',#14859);
#1745=PLANE('',#14864);
#1746=PLANE('',#14873);
#1747=PLANE('',#14877);
#1748=PLANE('',#14878);
#1749=PLANE('',#14880);
#1750=PLANE('',#14885);
#1751=PLANE('',#14888);
#1752=PLANE('',#14893);
#1753=PLANE('',#14973);
#1754=PLANE('',#14974);
#1755=PLANE('',#14975);
#1756=PLANE('',#14982);
#1757=PLANE('',#14984);
#1758=PLANE('',#14985);
#1759=PLANE('',#14986);
#1760=PLANE('',#14987);
#1761=PLANE('',#14990);
#1762=PLANE('',#14991);
#1763=PLANE('',#14992);
#1764=PLANE('',#14993);
#1765=PLANE('',#14994);
#1766=PLANE('',#14995);
#1767=PLANE('',#14996);
#1768=PLANE('',#14997);
#1769=PLANE('',#14999);
#1770=PLANE('',#15000);
#1771=PLANE('',#15001);
#1772=PLANE('',#15002);
#1773=PLANE('',#15003);
#1774=PLANE('',#15004);
#1775=PLANE('',#15006);
#1776=PLANE('',#15007);
#1777=PLANE('',#15008);
#1778=PLANE('',#15009);
#1779=PLANE('',#15010);
#1780=PLANE('',#15011);
#1781=PLANE('',#15016);
#1782=PLANE('',#15026);
#1783=PLANE('',#15029);
#1784=PLANE('',#15037);
#1785=PLANE('',#15038);
#1786=PLANE('',#15046);
#1787=PLANE('',#15047);
#1788=PLANE('',#15055);
#1789=PLANE('',#15056);
#1790=PLANE('',#15064);
#1791=PLANE('',#15065);
#1792=PLANE('',#15073);
#1793=PLANE('',#15074);
#1794=PLANE('',#15079);
#1795=PLANE('',#15089);
#1796=PLANE('',#15092);
#1797=PLANE('',#15100);
#1798=PLANE('',#15101);
#1799=PLANE('',#15109);
#1800=PLANE('',#15110);
#1801=PLANE('',#15118);
#1802=PLANE('',#15119);
#1803=PLANE('',#15127);
#1804=PLANE('',#15128);
#1805=PLANE('',#15130);
#1806=PLANE('',#15138);
#1807=PLANE('',#15146);
#1808=PLANE('',#15147);
#1809=PLANE('',#15148);
#1810=PLANE('',#15149);
#1811=PLANE('',#15150);
#1812=PLANE('',#15151);
#1813=PLANE('',#15152);
#1814=PLANE('',#15153);
#1815=PLANE('',#15154);
#1816=PLANE('',#15237);
#1817=PLANE('',#15238);
#1818=PLANE('',#15239);
#1819=PLANE('',#15240);
#1820=PLANE('',#15241);
#1821=PLANE('',#15242);
#1822=PLANE('',#15253);
#1823=PLANE('',#15254);
#1824=PLANE('',#15255);
#1825=PLANE('',#15256);
#1826=PLANE('',#15257);
#1827=PLANE('',#15258);
#1828=PLANE('',#15269);
#1829=PLANE('',#15270);
#1830=PLANE('',#15271);
#1831=PLANE('',#15272);
#1832=PLANE('',#15273);
#1833=PLANE('',#15274);
#1834=PLANE('',#15279);
#1835=PLANE('',#15280);
#1836=PLANE('',#15281);
#1837=PLANE('',#15282);
#1838=PLANE('',#15283);
#1839=PLANE('',#15284);
#1840=PLANE('',#15289);
#1841=PLANE('',#15290);
#1842=PLANE('',#15295);
#1843=PLANE('',#15298);
#1844=PLANE('',#15306);
#1845=PLANE('',#15307);
#1846=PLANE('',#15315);
#1847=PLANE('',#15316);
#1848=PLANE('',#15319);
#1849=PLANE('',#15321);
#1850=PLANE('',#15322);
#1851=PLANE('',#15324);
#1852=PLANE('',#15325);
#1853=PLANE('',#15326);
#1854=PLANE('',#15331);
#1855=PLANE('',#15335);
#1856=PLANE('',#15339);
#1857=PLANE('',#15343);
#1858=PLANE('',#15347);
#1859=PLANE('',#15351);
#1860=PLANE('',#15354);
#1861=PLANE('',#15355);
#1862=PLANE('',#15358);
#1863=PLANE('',#15359);
#1864=PLANE('',#15364);
#1865=PLANE('',#15370);
#1866=PLANE('',#15371);
#1867=PLANE('',#15372);
#1868=PLANE('',#15373);
#1869=PLANE('',#15374);
#1870=PLANE('',#15375);
#1871=PLANE('',#15376);
#1872=PLANE('',#15377);
#1873=PLANE('',#15378);
#1874=PLANE('',#15380);
#1875=PLANE('',#15388);
#1876=PLANE('',#15411);
#1877=PLANE('',#15414);
#1878=PLANE('',#15419);
#1879=PLANE('',#15420);
#1880=PLANE('',#15427);
#1881=PLANE('',#15428);
#1882=PLANE('',#15436);
#1883=PLANE('',#15437);
#1884=PLANE('',#15445);
#1885=PLANE('',#15446);
#1886=PLANE('',#15454);
#1887=PLANE('',#15455);
#1888=PLANE('',#15460);
#1889=PLANE('',#15461);
#1890=FACE_OUTER_BOUND('',#2667,.T.);
#1891=FACE_OUTER_BOUND('',#2668,.T.);
#1892=FACE_OUTER_BOUND('',#2669,.T.);
#1893=FACE_OUTER_BOUND('',#2670,.T.);
#1894=FACE_OUTER_BOUND('',#2671,.T.);
#1895=FACE_OUTER_BOUND('',#2672,.T.);
#1896=FACE_OUTER_BOUND('',#2673,.T.);
#1897=FACE_OUTER_BOUND('',#2674,.T.);
#1898=FACE_OUTER_BOUND('',#2675,.T.);
#1899=FACE_OUTER_BOUND('',#2676,.T.);
#1900=FACE_OUTER_BOUND('',#2677,.T.);
#1901=FACE_OUTER_BOUND('',#2678,.T.);
#1902=FACE_OUTER_BOUND('',#2679,.T.);
#1903=FACE_OUTER_BOUND('',#2680,.T.);
#1904=FACE_OUTER_BOUND('',#2681,.T.);
#1905=FACE_OUTER_BOUND('',#2682,.T.);
#1906=FACE_OUTER_BOUND('',#2683,.T.);
#1907=FACE_OUTER_BOUND('',#2696,.T.);
#1908=FACE_OUTER_BOUND('',#2709,.T.);
#1909=FACE_OUTER_BOUND('',#2710,.T.);
#1910=FACE_OUTER_BOUND('',#2711,.T.);
#1911=FACE_OUTER_BOUND('',#2712,.T.);
#1912=FACE_OUTER_BOUND('',#2713,.T.);
#1913=FACE_OUTER_BOUND('',#2714,.T.);
#1914=FACE_OUTER_BOUND('',#2715,.T.);
#1915=FACE_OUTER_BOUND('',#2716,.T.);
#1916=FACE_OUTER_BOUND('',#2717,.T.);
#1917=FACE_OUTER_BOUND('',#2718,.T.);
#1918=FACE_OUTER_BOUND('',#2719,.T.);
#1919=FACE_OUTER_BOUND('',#2720,.T.);
#1920=FACE_OUTER_BOUND('',#2721,.T.);
#1921=FACE_OUTER_BOUND('',#2722,.T.);
#1922=FACE_OUTER_BOUND('',#2723,.T.);
#1923=FACE_OUTER_BOUND('',#2724,.T.);
#1924=FACE_OUTER_BOUND('',#2725,.T.);
#1925=FACE_OUTER_BOUND('',#2726,.T.);
#1926=FACE_OUTER_BOUND('',#2727,.T.);
#1927=FACE_OUTER_BOUND('',#2728,.T.);
#1928=FACE_OUTER_BOUND('',#2729,.T.);
#1929=FACE_OUTER_BOUND('',#2734,.T.);
#1930=FACE_OUTER_BOUND('',#2735,.T.);
#1931=FACE_OUTER_BOUND('',#2736,.T.);
#1932=FACE_OUTER_BOUND('',#2737,.T.);
#1933=FACE_OUTER_BOUND('',#2742,.T.);
#1934=FACE_OUTER_BOUND('',#2743,.T.);
#1935=FACE_OUTER_BOUND('',#2748,.T.);
#1936=FACE_OUTER_BOUND('',#2749,.T.);
#1937=FACE_OUTER_BOUND('',#2750,.T.);
#1938=FACE_OUTER_BOUND('',#2755,.T.);
#1939=FACE_OUTER_BOUND('',#2756,.T.);
#1940=FACE_OUTER_BOUND('',#2757,.T.);
#1941=FACE_OUTER_BOUND('',#2758,.T.);
#1942=FACE_OUTER_BOUND('',#2759,.T.);
#1943=FACE_OUTER_BOUND('',#2760,.T.);
#1944=FACE_OUTER_BOUND('',#2761,.T.);
#1945=FACE_OUTER_BOUND('',#2762,.T.);
#1946=FACE_OUTER_BOUND('',#2763,.T.);
#1947=FACE_OUTER_BOUND('',#2768,.T.);
#1948=FACE_OUTER_BOUND('',#2769,.T.);
#1949=FACE_OUTER_BOUND('',#2770,.T.);
#1950=FACE_OUTER_BOUND('',#2771,.T.);
#1951=FACE_OUTER_BOUND('',#2776,.T.);
#1952=FACE_OUTER_BOUND('',#2777,.T.);
#1953=FACE_OUTER_BOUND('',#2782,.T.);
#1954=FACE_OUTER_BOUND('',#2783,.T.);
#1955=FACE_OUTER_BOUND('',#2784,.T.);
#1956=FACE_OUTER_BOUND('',#2789,.T.);
#1957=FACE_OUTER_BOUND('',#2790,.T.);
#1958=FACE_OUTER_BOUND('',#2791,.T.);
#1959=FACE_OUTER_BOUND('',#2792,.T.);
#1960=FACE_OUTER_BOUND('',#2793,.T.);
#1961=FACE_OUTER_BOUND('',#2794,.T.);
#1962=FACE_OUTER_BOUND('',#2799,.T.);
#1963=FACE_OUTER_BOUND('',#2804,.T.);
#1964=FACE_OUTER_BOUND('',#2805,.T.);
#1965=FACE_OUTER_BOUND('',#2806,.T.);
#1966=FACE_OUTER_BOUND('',#2807,.T.);
#1967=FACE_OUTER_BOUND('',#2808,.T.);
#1968=FACE_OUTER_BOUND('',#2810,.T.);
#1969=FACE_OUTER_BOUND('',#2811,.T.);
#1970=FACE_OUTER_BOUND('',#2812,.T.);
#1971=FACE_OUTER_BOUND('',#2814,.T.);
#1972=FACE_OUTER_BOUND('',#2816,.T.);
#1973=FACE_OUTER_BOUND('',#2817,.T.);
#1974=FACE_OUTER_BOUND('',#2818,.T.);
#1975=FACE_OUTER_BOUND('',#2820,.T.);
#1976=FACE_OUTER_BOUND('',#2822,.T.);
#1977=FACE_OUTER_BOUND('',#2823,.T.);
#1978=FACE_OUTER_BOUND('',#2824,.T.);
#1979=FACE_OUTER_BOUND('',#2826,.T.);
#1980=FACE_OUTER_BOUND('',#2828,.T.);
#1981=FACE_OUTER_BOUND('',#2829,.T.);
#1982=FACE_OUTER_BOUND('',#2830,.T.);
#1983=FACE_OUTER_BOUND('',#2831,.T.);
#1984=FACE_OUTER_BOUND('',#2832,.T.);
#1985=FACE_OUTER_BOUND('',#2833,.T.);
#1986=FACE_OUTER_BOUND('',#2838,.T.);
#1987=FACE_OUTER_BOUND('',#2843,.T.);
#1988=FACE_OUTER_BOUND('',#2844,.T.);
#1989=FACE_OUTER_BOUND('',#2845,.T.);
#1990=FACE_OUTER_BOUND('',#2846,.T.);
#1991=FACE_OUTER_BOUND('',#2847,.T.);
#1992=FACE_OUTER_BOUND('',#2849,.T.);
#1993=FACE_OUTER_BOUND('',#2850,.T.);
#1994=FACE_OUTER_BOUND('',#2851,.T.);
#1995=FACE_OUTER_BOUND('',#2853,.T.);
#1996=FACE_OUTER_BOUND('',#2855,.T.);
#1997=FACE_OUTER_BOUND('',#2856,.T.);
#1998=FACE_OUTER_BOUND('',#2857,.T.);
#1999=FACE_OUTER_BOUND('',#2859,.T.);
#2000=FACE_OUTER_BOUND('',#2861,.T.);
#2001=FACE_OUTER_BOUND('',#2862,.T.);
#2002=FACE_OUTER_BOUND('',#2863,.T.);
#2003=FACE_OUTER_BOUND('',#2865,.T.);
#2004=FACE_OUTER_BOUND('',#2867,.T.);
#2005=FACE_OUTER_BOUND('',#2868,.T.);
#2006=FACE_OUTER_BOUND('',#2869,.T.);
#2007=FACE_OUTER_BOUND('',#2871,.T.);
#2008=FACE_OUTER_BOUND('',#2876,.T.);
#2009=FACE_OUTER_BOUND('',#2877,.T.);
#2010=FACE_OUTER_BOUND('',#2879,.T.);
#2011=FACE_OUTER_BOUND('',#2880,.T.);
#2012=FACE_OUTER_BOUND('',#2881,.T.);
#2013=FACE_OUTER_BOUND('',#2883,.T.);
#2014=FACE_OUTER_BOUND('',#2884,.T.);
#2015=FACE_OUTER_BOUND('',#2885,.T.);
#2016=FACE_OUTER_BOUND('',#2886,.T.);
#2017=FACE_OUTER_BOUND('',#2887,.T.);
#2018=FACE_OUTER_BOUND('',#2888,.T.);
#2019=FACE_OUTER_BOUND('',#2889,.T.);
#2020=FACE_OUTER_BOUND('',#2894,.T.);
#2021=FACE_OUTER_BOUND('',#2896,.T.);
#2022=FACE_OUTER_BOUND('',#2899,.T.);
#2023=FACE_OUTER_BOUND('',#2900,.T.);
#2024=FACE_OUTER_BOUND('',#2901,.T.);
#2025=FACE_OUTER_BOUND('',#2902,.T.);
#2026=FACE_OUTER_BOUND('',#2903,.T.);
#2027=FACE_OUTER_BOUND('',#2907,.T.);
#2028=FACE_OUTER_BOUND('',#2908,.T.);
#2029=FACE_OUTER_BOUND('',#2909,.T.);
#2030=FACE_OUTER_BOUND('',#2910,.T.);
#2031=FACE_OUTER_BOUND('',#2914,.T.);
#2032=FACE_OUTER_BOUND('',#2916,.T.);
#2033=FACE_OUTER_BOUND('',#2917,.T.);
#2034=FACE_OUTER_BOUND('',#2918,.T.);
#2035=FACE_OUTER_BOUND('',#2919,.T.);
#2036=FACE_OUTER_BOUND('',#2920,.T.);
#2037=FACE_OUTER_BOUND('',#2922,.T.);
#2038=FACE_OUTER_BOUND('',#2923,.T.);
#2039=FACE_OUTER_BOUND('',#2924,.T.);
#2040=FACE_OUTER_BOUND('',#2925,.T.);
#2041=FACE_OUTER_BOUND('',#2926,.T.);
#2042=FACE_OUTER_BOUND('',#2927,.T.);
#2043=FACE_OUTER_BOUND('',#2928,.T.);
#2044=FACE_OUTER_BOUND('',#2929,.T.);
#2045=FACE_OUTER_BOUND('',#2930,.T.);
#2046=FACE_OUTER_BOUND('',#2934,.T.);
#2047=FACE_OUTER_BOUND('',#2935,.T.);
#2048=FACE_OUTER_BOUND('',#2936,.T.);
#2049=FACE_OUTER_BOUND('',#2937,.T.);
#2050=FACE_OUTER_BOUND('',#2941,.T.);
#2051=FACE_OUTER_BOUND('',#2943,.T.);
#2052=FACE_OUTER_BOUND('',#2944,.T.);
#2053=FACE_OUTER_BOUND('',#2945,.T.);
#2054=FACE_OUTER_BOUND('',#2946,.T.);
#2055=FACE_OUTER_BOUND('',#2947,.T.);
#2056=FACE_OUTER_BOUND('',#2949,.T.);
#2057=FACE_OUTER_BOUND('',#2950,.T.);
#2058=FACE_OUTER_BOUND('',#2951,.T.);
#2059=FACE_OUTER_BOUND('',#2952,.T.);
#2060=FACE_OUTER_BOUND('',#2953,.T.);
#2061=FACE_OUTER_BOUND('',#2954,.T.);
#2062=FACE_OUTER_BOUND('',#2955,.T.);
#2063=FACE_OUTER_BOUND('',#2957,.T.);
#2064=FACE_OUTER_BOUND('',#2962,.T.);
#2065=FACE_OUTER_BOUND('',#2963,.T.);
#2066=FACE_OUTER_BOUND('',#2965,.T.);
#2067=FACE_OUTER_BOUND('',#2966,.T.);
#2068=FACE_OUTER_BOUND('',#2967,.T.);
#2069=FACE_OUTER_BOUND('',#2969,.T.);
#2070=FACE_OUTER_BOUND('',#2970,.T.);
#2071=FACE_OUTER_BOUND('',#2971,.T.);
#2072=FACE_OUTER_BOUND('',#2972,.T.);
#2073=FACE_OUTER_BOUND('',#2973,.T.);
#2074=FACE_OUTER_BOUND('',#2974,.T.);
#2075=FACE_OUTER_BOUND('',#2975,.T.);
#2076=FACE_OUTER_BOUND('',#2980,.T.);
#2077=FACE_OUTER_BOUND('',#2982,.T.);
#2078=FACE_OUTER_BOUND('',#2985,.T.);
#2079=FACE_OUTER_BOUND('',#2986,.T.);
#2080=FACE_OUTER_BOUND('',#2987,.T.);
#2081=FACE_OUTER_BOUND('',#2988,.T.);
#2082=FACE_OUTER_BOUND('',#2989,.T.);
#2083=FACE_OUTER_BOUND('',#2993,.T.);
#2084=FACE_OUTER_BOUND('',#2994,.T.);
#2085=FACE_OUTER_BOUND('',#2995,.T.);
#2086=FACE_OUTER_BOUND('',#2996,.T.);
#2087=FACE_OUTER_BOUND('',#3000,.T.);
#2088=FACE_OUTER_BOUND('',#3002,.T.);
#2089=FACE_OUTER_BOUND('',#3003,.T.);
#2090=FACE_OUTER_BOUND('',#3004,.T.);
#2091=FACE_OUTER_BOUND('',#3005,.T.);
#2092=FACE_OUTER_BOUND('',#3006,.T.);
#2093=FACE_OUTER_BOUND('',#3008,.T.);
#2094=FACE_OUTER_BOUND('',#3009,.T.);
#2095=FACE_OUTER_BOUND('',#3010,.T.);
#2096=FACE_OUTER_BOUND('',#3011,.T.);
#2097=FACE_OUTER_BOUND('',#3012,.T.);
#2098=FACE_OUTER_BOUND('',#3013,.T.);
#2099=FACE_OUTER_BOUND('',#3014,.T.);
#2100=FACE_OUTER_BOUND('',#3015,.T.);
#2101=FACE_OUTER_BOUND('',#3016,.T.);
#2102=FACE_OUTER_BOUND('',#3020,.T.);
#2103=FACE_OUTER_BOUND('',#3021,.T.);
#2104=FACE_OUTER_BOUND('',#3022,.T.);
#2105=FACE_OUTER_BOUND('',#3023,.T.);
#2106=FACE_OUTER_BOUND('',#3027,.T.);
#2107=FACE_OUTER_BOUND('',#3029,.T.);
#2108=FACE_OUTER_BOUND('',#3030,.T.);
#2109=FACE_OUTER_BOUND('',#3031,.T.);
#2110=FACE_OUTER_BOUND('',#3032,.T.);
#2111=FACE_OUTER_BOUND('',#3033,.T.);
#2112=FACE_OUTER_BOUND('',#3035,.T.);
#2113=FACE_OUTER_BOUND('',#3036,.T.);
#2114=FACE_OUTER_BOUND('',#3037,.T.);
#2115=FACE_OUTER_BOUND('',#3038,.T.);
#2116=FACE_OUTER_BOUND('',#3039,.T.);
#2117=FACE_OUTER_BOUND('',#3040,.T.);
#2118=FACE_OUTER_BOUND('',#3041,.T.);
#2119=FACE_OUTER_BOUND('',#3042,.T.);
#2120=FACE_OUTER_BOUND('',#3043,.T.);
#2121=FACE_OUTER_BOUND('',#3044,.T.);
#2122=FACE_OUTER_BOUND('',#3045,.T.);
#2123=FACE_OUTER_BOUND('',#3046,.T.);
#2124=FACE_OUTER_BOUND('',#3047,.T.);
#2125=FACE_OUTER_BOUND('',#3048,.T.);
#2126=FACE_OUTER_BOUND('',#3049,.T.);
#2127=FACE_OUTER_BOUND('',#3051,.T.);
#2128=FACE_OUTER_BOUND('',#3052,.T.);
#2129=FACE_OUTER_BOUND('',#3053,.T.);
#2130=FACE_OUTER_BOUND('',#3054,.T.);
#2131=FACE_OUTER_BOUND('',#3055,.T.);
#2132=FACE_OUTER_BOUND('',#3056,.T.);
#2133=FACE_OUTER_BOUND('',#3057,.T.);
#2134=FACE_OUTER_BOUND('',#3058,.T.);
#2135=FACE_OUTER_BOUND('',#3059,.T.);
#2136=FACE_OUTER_BOUND('',#3060,.T.);
#2137=FACE_OUTER_BOUND('',#3061,.T.);
#2138=FACE_OUTER_BOUND('',#3062,.T.);
#2139=FACE_OUTER_BOUND('',#3063,.T.);
#2140=FACE_OUTER_BOUND('',#3064,.T.);
#2141=FACE_OUTER_BOUND('',#3065,.T.);
#2142=FACE_OUTER_BOUND('',#3066,.T.);
#2143=FACE_OUTER_BOUND('',#3067,.T.);
#2144=FACE_OUTER_BOUND('',#3068,.T.);
#2145=FACE_OUTER_BOUND('',#3069,.T.);
#2146=FACE_OUTER_BOUND('',#3080,.T.);
#2147=FACE_OUTER_BOUND('',#3081,.T.);
#2148=FACE_OUTER_BOUND('',#3082,.T.);
#2149=FACE_OUTER_BOUND('',#3083,.T.);
#2150=FACE_OUTER_BOUND('',#3084,.T.);
#2151=FACE_OUTER_BOUND('',#3085,.T.);
#2152=FACE_OUTER_BOUND('',#3086,.T.);
#2153=FACE_OUTER_BOUND('',#3087,.T.);
#2154=FACE_OUTER_BOUND('',#3088,.T.);
#2155=FACE_OUTER_BOUND('',#3099,.T.);
#2156=FACE_OUTER_BOUND('',#3100,.T.);
#2157=FACE_OUTER_BOUND('',#3101,.T.);
#2158=FACE_OUTER_BOUND('',#3102,.T.);
#2159=FACE_OUTER_BOUND('',#3103,.T.);
#2160=FACE_OUTER_BOUND('',#3104,.T.);
#2161=FACE_OUTER_BOUND('',#3105,.T.);
#2162=FACE_OUTER_BOUND('',#3111,.T.);
#2163=FACE_OUTER_BOUND('',#3117,.T.);
#2164=FACE_OUTER_BOUND('',#3119,.T.);
#2165=FACE_OUTER_BOUND('',#3120,.T.);
#2166=FACE_OUTER_BOUND('',#3121,.T.);
#2167=FACE_OUTER_BOUND('',#3122,.T.);
#2168=FACE_OUTER_BOUND('',#3123,.T.);
#2169=FACE_OUTER_BOUND('',#3125,.T.);
#2170=FACE_OUTER_BOUND('',#3126,.T.);
#2171=FACE_OUTER_BOUND('',#3127,.T.);
#2172=FACE_OUTER_BOUND('',#3128,.T.);
#2173=FACE_OUTER_BOUND('',#3129,.T.);
#2174=FACE_OUTER_BOUND('',#3131,.T.);
#2175=FACE_OUTER_BOUND('',#3132,.T.);
#2176=FACE_OUTER_BOUND('',#3133,.T.);
#2177=FACE_OUTER_BOUND('',#3134,.T.);
#2178=FACE_OUTER_BOUND('',#3135,.T.);
#2179=FACE_OUTER_BOUND('',#3137,.T.);
#2180=FACE_OUTER_BOUND('',#3138,.T.);
#2181=FACE_OUTER_BOUND('',#3139,.T.);
#2182=FACE_OUTER_BOUND('',#3140,.T.);
#2183=FACE_OUTER_BOUND('',#3141,.T.);
#2184=FACE_OUTER_BOUND('',#3142,.T.);
#2185=FACE_OUTER_BOUND('',#3143,.T.);
#2186=FACE_OUTER_BOUND('',#3144,.T.);
#2187=FACE_OUTER_BOUND('',#3145,.T.);
#2188=FACE_OUTER_BOUND('',#3146,.T.);
#2189=FACE_OUTER_BOUND('',#3147,.T.);
#2190=FACE_OUTER_BOUND('',#3153,.T.);
#2191=FACE_OUTER_BOUND('',#3159,.T.);
#2192=FACE_OUTER_BOUND('',#3161,.T.);
#2193=FACE_OUTER_BOUND('',#3162,.T.);
#2194=FACE_OUTER_BOUND('',#3163,.T.);
#2195=FACE_OUTER_BOUND('',#3164,.T.);
#2196=FACE_OUTER_BOUND('',#3165,.T.);
#2197=FACE_OUTER_BOUND('',#3167,.T.);
#2198=FACE_OUTER_BOUND('',#3168,.T.);
#2199=FACE_OUTER_BOUND('',#3169,.T.);
#2200=FACE_OUTER_BOUND('',#3170,.T.);
#2201=FACE_OUTER_BOUND('',#3171,.T.);
#2202=FACE_OUTER_BOUND('',#3173,.T.);
#2203=FACE_OUTER_BOUND('',#3174,.T.);
#2204=FACE_OUTER_BOUND('',#3175,.T.);
#2205=FACE_OUTER_BOUND('',#3176,.T.);
#2206=FACE_OUTER_BOUND('',#3177,.T.);
#2207=FACE_OUTER_BOUND('',#3179,.T.);
#2208=FACE_OUTER_BOUND('',#3180,.T.);
#2209=FACE_OUTER_BOUND('',#3181,.T.);
#2210=FACE_OUTER_BOUND('',#3182,.T.);
#2211=FACE_OUTER_BOUND('',#3183,.T.);
#2212=FACE_OUTER_BOUND('',#3184,.T.);
#2213=FACE_OUTER_BOUND('',#3185,.T.);
#2214=FACE_OUTER_BOUND('',#3186,.T.);
#2215=FACE_OUTER_BOUND('',#3187,.T.);
#2216=FACE_OUTER_BOUND('',#3188,.T.);
#2217=FACE_OUTER_BOUND('',#3189,.T.);
#2218=FACE_OUTER_BOUND('',#3195,.T.);
#2219=FACE_OUTER_BOUND('',#3201,.T.);
#2220=FACE_OUTER_BOUND('',#3203,.T.);
#2221=FACE_OUTER_BOUND('',#3204,.T.);
#2222=FACE_OUTER_BOUND('',#3205,.T.);
#2223=FACE_OUTER_BOUND('',#3206,.T.);
#2224=FACE_OUTER_BOUND('',#3207,.T.);
#2225=FACE_OUTER_BOUND('',#3209,.T.);
#2226=FACE_OUTER_BOUND('',#3210,.T.);
#2227=FACE_OUTER_BOUND('',#3211,.T.);
#2228=FACE_OUTER_BOUND('',#3212,.T.);
#2229=FACE_OUTER_BOUND('',#3213,.T.);
#2230=FACE_OUTER_BOUND('',#3215,.T.);
#2231=FACE_OUTER_BOUND('',#3216,.T.);
#2232=FACE_OUTER_BOUND('',#3217,.T.);
#2233=FACE_OUTER_BOUND('',#3218,.T.);
#2234=FACE_OUTER_BOUND('',#3219,.T.);
#2235=FACE_OUTER_BOUND('',#3221,.T.);
#2236=FACE_OUTER_BOUND('',#3222,.T.);
#2237=FACE_OUTER_BOUND('',#3223,.T.);
#2238=FACE_OUTER_BOUND('',#3224,.T.);
#2239=FACE_OUTER_BOUND('',#3225,.T.);
#2240=FACE_OUTER_BOUND('',#3226,.T.);
#2241=FACE_OUTER_BOUND('',#3227,.T.);
#2242=FACE_OUTER_BOUND('',#3228,.T.);
#2243=FACE_OUTER_BOUND('',#3229,.T.);
#2244=FACE_OUTER_BOUND('',#3230,.T.);
#2245=FACE_OUTER_BOUND('',#3231,.T.);
#2246=FACE_OUTER_BOUND('',#3237,.T.);
#2247=FACE_OUTER_BOUND('',#3243,.T.);
#2248=FACE_OUTER_BOUND('',#3245,.T.);
#2249=FACE_OUTER_BOUND('',#3246,.T.);
#2250=FACE_OUTER_BOUND('',#3247,.T.);
#2251=FACE_OUTER_BOUND('',#3248,.T.);
#2252=FACE_OUTER_BOUND('',#3249,.T.);
#2253=FACE_OUTER_BOUND('',#3251,.T.);
#2254=FACE_OUTER_BOUND('',#3252,.T.);
#2255=FACE_OUTER_BOUND('',#3253,.T.);
#2256=FACE_OUTER_BOUND('',#3254,.T.);
#2257=FACE_OUTER_BOUND('',#3255,.T.);
#2258=FACE_OUTER_BOUND('',#3257,.T.);
#2259=FACE_OUTER_BOUND('',#3258,.T.);
#2260=FACE_OUTER_BOUND('',#3259,.T.);
#2261=FACE_OUTER_BOUND('',#3260,.T.);
#2262=FACE_OUTER_BOUND('',#3261,.T.);
#2263=FACE_OUTER_BOUND('',#3263,.T.);
#2264=FACE_OUTER_BOUND('',#3264,.T.);
#2265=FACE_OUTER_BOUND('',#3265,.T.);
#2266=FACE_OUTER_BOUND('',#3266,.T.);
#2267=FACE_OUTER_BOUND('',#3267,.T.);
#2268=FACE_OUTER_BOUND('',#3268,.T.);
#2269=FACE_OUTER_BOUND('',#3269,.T.);
#2270=FACE_OUTER_BOUND('',#3270,.T.);
#2271=FACE_OUTER_BOUND('',#3271,.T.);
#2272=FACE_OUTER_BOUND('',#3272,.T.);
#2273=FACE_OUTER_BOUND('',#3273,.T.);
#2274=FACE_OUTER_BOUND('',#3274,.T.);
#2275=FACE_OUTER_BOUND('',#3285,.T.);
#2276=FACE_OUTER_BOUND('',#3286,.T.);
#2277=FACE_OUTER_BOUND('',#3287,.T.);
#2278=FACE_OUTER_BOUND('',#3288,.T.);
#2279=FACE_OUTER_BOUND('',#3289,.T.);
#2280=FACE_OUTER_BOUND('',#3290,.T.);
#2281=FACE_OUTER_BOUND('',#3291,.T.);
#2282=FACE_OUTER_BOUND('',#3292,.T.);
#2283=FACE_OUTER_BOUND('',#3303,.T.);
#2284=FACE_OUTER_BOUND('',#3304,.T.);
#2285=FACE_OUTER_BOUND('',#3305,.T.);
#2286=FACE_OUTER_BOUND('',#3306,.T.);
#2287=FACE_OUTER_BOUND('',#3307,.T.);
#2288=FACE_OUTER_BOUND('',#3308,.T.);
#2289=FACE_OUTER_BOUND('',#3309,.T.);
#2290=FACE_OUTER_BOUND('',#3315,.T.);
#2291=FACE_OUTER_BOUND('',#3321,.T.);
#2292=FACE_OUTER_BOUND('',#3323,.T.);
#2293=FACE_OUTER_BOUND('',#3324,.T.);
#2294=FACE_OUTER_BOUND('',#3325,.T.);
#2295=FACE_OUTER_BOUND('',#3326,.T.);
#2296=FACE_OUTER_BOUND('',#3327,.T.);
#2297=FACE_OUTER_BOUND('',#3329,.T.);
#2298=FACE_OUTER_BOUND('',#3330,.T.);
#2299=FACE_OUTER_BOUND('',#3331,.T.);
#2300=FACE_OUTER_BOUND('',#3332,.T.);
#2301=FACE_OUTER_BOUND('',#3333,.T.);
#2302=FACE_OUTER_BOUND('',#3335,.T.);
#2303=FACE_OUTER_BOUND('',#3336,.T.);
#2304=FACE_OUTER_BOUND('',#3337,.T.);
#2305=FACE_OUTER_BOUND('',#3338,.T.);
#2306=FACE_OUTER_BOUND('',#3339,.T.);
#2307=FACE_OUTER_BOUND('',#3341,.T.);
#2308=FACE_OUTER_BOUND('',#3342,.T.);
#2309=FACE_OUTER_BOUND('',#3343,.T.);
#2310=FACE_OUTER_BOUND('',#3344,.T.);
#2311=FACE_OUTER_BOUND('',#3345,.T.);
#2312=FACE_OUTER_BOUND('',#3346,.T.);
#2313=FACE_OUTER_BOUND('',#3347,.T.);
#2314=FACE_OUTER_BOUND('',#3348,.T.);
#2315=FACE_OUTER_BOUND('',#3349,.T.);
#2316=FACE_OUTER_BOUND('',#3350,.T.);
#2317=FACE_OUTER_BOUND('',#3351,.T.);
#2318=FACE_OUTER_BOUND('',#3357,.T.);
#2319=FACE_OUTER_BOUND('',#3363,.T.);
#2320=FACE_OUTER_BOUND('',#3365,.T.);
#2321=FACE_OUTER_BOUND('',#3366,.T.);
#2322=FACE_OUTER_BOUND('',#3367,.T.);
#2323=FACE_OUTER_BOUND('',#3368,.T.);
#2324=FACE_OUTER_BOUND('',#3369,.T.);
#2325=FACE_OUTER_BOUND('',#3371,.T.);
#2326=FACE_OUTER_BOUND('',#3372,.T.);
#2327=FACE_OUTER_BOUND('',#3373,.T.);
#2328=FACE_OUTER_BOUND('',#3374,.T.);
#2329=FACE_OUTER_BOUND('',#3375,.T.);
#2330=FACE_OUTER_BOUND('',#3377,.T.);
#2331=FACE_OUTER_BOUND('',#3378,.T.);
#2332=FACE_OUTER_BOUND('',#3379,.T.);
#2333=FACE_OUTER_BOUND('',#3380,.T.);
#2334=FACE_OUTER_BOUND('',#3381,.T.);
#2335=FACE_OUTER_BOUND('',#3383,.T.);
#2336=FACE_OUTER_BOUND('',#3384,.T.);
#2337=FACE_OUTER_BOUND('',#3385,.T.);
#2338=FACE_OUTER_BOUND('',#3386,.T.);
#2339=FACE_OUTER_BOUND('',#3387,.T.);
#2340=FACE_OUTER_BOUND('',#3388,.T.);
#2341=FACE_OUTER_BOUND('',#3389,.T.);
#2342=FACE_OUTER_BOUND('',#3390,.T.);
#2343=FACE_OUTER_BOUND('',#3391,.T.);
#2344=FACE_OUTER_BOUND('',#3392,.T.);
#2345=FACE_OUTER_BOUND('',#3393,.T.);
#2346=FACE_OUTER_BOUND('',#3399,.T.);
#2347=FACE_OUTER_BOUND('',#3405,.T.);
#2348=FACE_OUTER_BOUND('',#3407,.T.);
#2349=FACE_OUTER_BOUND('',#3408,.T.);
#2350=FACE_OUTER_BOUND('',#3409,.T.);
#2351=FACE_OUTER_BOUND('',#3410,.T.);
#2352=FACE_OUTER_BOUND('',#3411,.T.);
#2353=FACE_OUTER_BOUND('',#3413,.T.);
#2354=FACE_OUTER_BOUND('',#3414,.T.);
#2355=FACE_OUTER_BOUND('',#3415,.T.);
#2356=FACE_OUTER_BOUND('',#3416,.T.);
#2357=FACE_OUTER_BOUND('',#3417,.T.);
#2358=FACE_OUTER_BOUND('',#3419,.T.);
#2359=FACE_OUTER_BOUND('',#3420,.T.);
#2360=FACE_OUTER_BOUND('',#3421,.T.);
#2361=FACE_OUTER_BOUND('',#3422,.T.);
#2362=FACE_OUTER_BOUND('',#3423,.T.);
#2363=FACE_OUTER_BOUND('',#3425,.T.);
#2364=FACE_OUTER_BOUND('',#3426,.T.);
#2365=FACE_OUTER_BOUND('',#3427,.T.);
#2366=FACE_OUTER_BOUND('',#3428,.T.);
#2367=FACE_OUTER_BOUND('',#3429,.T.);
#2368=FACE_OUTER_BOUND('',#3430,.T.);
#2369=FACE_OUTER_BOUND('',#3431,.T.);
#2370=FACE_OUTER_BOUND('',#3432,.T.);
#2371=FACE_OUTER_BOUND('',#3433,.T.);
#2372=FACE_OUTER_BOUND('',#3434,.T.);
#2373=FACE_OUTER_BOUND('',#3435,.T.);
#2374=FACE_OUTER_BOUND('',#3441,.T.);
#2375=FACE_OUTER_BOUND('',#3447,.T.);
#2376=FACE_OUTER_BOUND('',#3449,.T.);
#2377=FACE_OUTER_BOUND('',#3450,.T.);
#2378=FACE_OUTER_BOUND('',#3451,.T.);
#2379=FACE_OUTER_BOUND('',#3452,.T.);
#2380=FACE_OUTER_BOUND('',#3453,.T.);
#2381=FACE_OUTER_BOUND('',#3455,.T.);
#2382=FACE_OUTER_BOUND('',#3456,.T.);
#2383=FACE_OUTER_BOUND('',#3457,.T.);
#2384=FACE_OUTER_BOUND('',#3458,.T.);
#2385=FACE_OUTER_BOUND('',#3459,.T.);
#2386=FACE_OUTER_BOUND('',#3461,.T.);
#2387=FACE_OUTER_BOUND('',#3462,.T.);
#2388=FACE_OUTER_BOUND('',#3463,.T.);
#2389=FACE_OUTER_BOUND('',#3464,.T.);
#2390=FACE_OUTER_BOUND('',#3465,.T.);
#2391=FACE_OUTER_BOUND('',#3467,.T.);
#2392=FACE_OUTER_BOUND('',#3468,.T.);
#2393=FACE_OUTER_BOUND('',#3469,.T.);
#2394=FACE_OUTER_BOUND('',#3470,.T.);
#2395=FACE_OUTER_BOUND('',#3471,.T.);
#2396=FACE_OUTER_BOUND('',#3472,.T.);
#2397=FACE_OUTER_BOUND('',#3473,.T.);
#2398=FACE_OUTER_BOUND('',#3474,.T.);
#2399=FACE_OUTER_BOUND('',#3475,.T.);
#2400=FACE_OUTER_BOUND('',#3477,.T.);
#2401=FACE_OUTER_BOUND('',#3478,.T.);
#2402=FACE_OUTER_BOUND('',#3480,.T.);
#2403=FACE_OUTER_BOUND('',#3481,.T.);
#2404=FACE_OUTER_BOUND('',#3482,.T.);
#2405=FACE_OUTER_BOUND('',#3483,.T.);
#2406=FACE_OUTER_BOUND('',#3485,.T.);
#2407=FACE_OUTER_BOUND('',#3486,.T.);
#2408=FACE_OUTER_BOUND('',#3487,.T.);
#2409=FACE_OUTER_BOUND('',#3488,.T.);
#2410=FACE_OUTER_BOUND('',#3490,.T.);
#2411=FACE_OUTER_BOUND('',#3491,.T.);
#2412=FACE_OUTER_BOUND('',#3492,.T.);
#2413=FACE_OUTER_BOUND('',#3493,.T.);
#2414=FACE_OUTER_BOUND('',#3494,.T.);
#2415=FACE_OUTER_BOUND('',#3495,.T.);
#2416=FACE_OUTER_BOUND('',#3496,.T.);
#2417=FACE_OUTER_BOUND('',#3497,.T.);
#2418=FACE_OUTER_BOUND('',#3498,.T.);
#2419=FACE_OUTER_BOUND('',#3499,.T.);
#2420=FACE_OUTER_BOUND('',#3500,.T.);
#2421=FACE_OUTER_BOUND('',#3501,.T.);
#2422=FACE_OUTER_BOUND('',#3502,.T.);
#2423=FACE_OUTER_BOUND('',#3503,.T.);
#2424=FACE_OUTER_BOUND('',#3504,.T.);
#2425=FACE_OUTER_BOUND('',#3505,.T.);
#2426=FACE_OUTER_BOUND('',#3506,.T.);
#2427=FACE_OUTER_BOUND('',#3507,.T.);
#2428=FACE_OUTER_BOUND('',#3508,.T.);
#2429=FACE_OUTER_BOUND('',#3509,.T.);
#2430=FACE_OUTER_BOUND('',#3510,.T.);
#2431=FACE_OUTER_BOUND('',#3511,.T.);
#2432=FACE_OUTER_BOUND('',#3512,.T.);
#2433=FACE_OUTER_BOUND('',#3513,.T.);
#2434=FACE_OUTER_BOUND('',#3515,.T.);
#2435=FACE_OUTER_BOUND('',#3516,.T.);
#2436=FACE_OUTER_BOUND('',#3518,.T.);
#2437=FACE_OUTER_BOUND('',#3519,.T.);
#2438=FACE_OUTER_BOUND('',#3521,.T.);
#2439=FACE_OUTER_BOUND('',#3522,.T.);
#2440=FACE_OUTER_BOUND('',#3524,.T.);
#2441=FACE_OUTER_BOUND('',#3525,.T.);
#2442=FACE_OUTER_BOUND('',#3527,.T.);
#2443=FACE_OUTER_BOUND('',#3528,.T.);
#2444=FACE_OUTER_BOUND('',#3529,.T.);
#2445=FACE_OUTER_BOUND('',#3530,.T.);
#2446=FACE_OUTER_BOUND('',#3531,.T.);
#2447=FACE_OUTER_BOUND('',#3532,.T.);
#2448=FACE_OUTER_BOUND('',#3533,.T.);
#2449=FACE_OUTER_BOUND('',#3534,.T.);
#2450=FACE_OUTER_BOUND('',#3535,.T.);
#2451=FACE_OUTER_BOUND('',#3536,.T.);
#2452=FACE_OUTER_BOUND('',#3537,.T.);
#2453=FACE_OUTER_BOUND('',#3538,.T.);
#2454=FACE_OUTER_BOUND('',#3539,.T.);
#2455=FACE_OUTER_BOUND('',#3540,.T.);
#2456=FACE_OUTER_BOUND('',#3541,.T.);
#2457=FACE_OUTER_BOUND('',#3550,.T.);
#2458=FACE_OUTER_BOUND('',#3551,.T.);
#2459=FACE_OUTER_BOUND('',#3552,.T.);
#2460=FACE_OUTER_BOUND('',#3553,.T.);
#2461=FACE_OUTER_BOUND('',#3554,.T.);
#2462=FACE_OUTER_BOUND('',#3555,.T.);
#2463=FACE_OUTER_BOUND('',#3556,.T.);
#2464=FACE_OUTER_BOUND('',#3565,.T.);
#2465=FACE_OUTER_BOUND('',#3566,.T.);
#2466=FACE_OUTER_BOUND('',#3567,.T.);
#2467=FACE_OUTER_BOUND('',#3568,.T.);
#2468=FACE_OUTER_BOUND('',#3569,.T.);
#2469=FACE_OUTER_BOUND('',#3570,.T.);
#2470=FACE_OUTER_BOUND('',#3571,.T.);
#2471=FACE_OUTER_BOUND('',#3572,.T.);
#2472=FACE_OUTER_BOUND('',#3573,.T.);
#2473=FACE_OUTER_BOUND('',#3574,.T.);
#2474=FACE_OUTER_BOUND('',#3575,.T.);
#2475=FACE_OUTER_BOUND('',#3576,.T.);
#2476=FACE_OUTER_BOUND('',#3577,.T.);
#2477=FACE_OUTER_BOUND('',#3578,.T.);
#2478=FACE_OUTER_BOUND('',#3579,.T.);
#2479=FACE_OUTER_BOUND('',#3580,.T.);
#2480=FACE_OUTER_BOUND('',#3581,.T.);
#2481=FACE_OUTER_BOUND('',#3582,.T.);
#2482=FACE_OUTER_BOUND('',#3583,.T.);
#2483=FACE_OUTER_BOUND('',#3584,.T.);
#2484=FACE_OUTER_BOUND('',#3585,.T.);
#2485=FACE_OUTER_BOUND('',#3586,.T.);
#2486=FACE_OUTER_BOUND('',#3587,.T.);
#2487=FACE_OUTER_BOUND('',#3588,.T.);
#2488=FACE_OUTER_BOUND('',#3593,.T.);
#2489=FACE_OUTER_BOUND('',#3598,.T.);
#2490=FACE_OUTER_BOUND('',#3599,.T.);
#2491=FACE_OUTER_BOUND('',#3600,.T.);
#2492=FACE_OUTER_BOUND('',#3601,.T.);
#2493=FACE_OUTER_BOUND('',#3602,.T.);
#2494=FACE_OUTER_BOUND('',#3604,.T.);
#2495=FACE_OUTER_BOUND('',#3605,.T.);
#2496=FACE_OUTER_BOUND('',#3606,.T.);
#2497=FACE_OUTER_BOUND('',#3608,.T.);
#2498=FACE_OUTER_BOUND('',#3610,.T.);
#2499=FACE_OUTER_BOUND('',#3611,.T.);
#2500=FACE_OUTER_BOUND('',#3612,.T.);
#2501=FACE_OUTER_BOUND('',#3614,.T.);
#2502=FACE_OUTER_BOUND('',#3616,.T.);
#2503=FACE_OUTER_BOUND('',#3617,.T.);
#2504=FACE_OUTER_BOUND('',#3618,.T.);
#2505=FACE_OUTER_BOUND('',#3620,.T.);
#2506=FACE_OUTER_BOUND('',#3622,.T.);
#2507=FACE_OUTER_BOUND('',#3623,.T.);
#2508=FACE_OUTER_BOUND('',#3624,.T.);
#2509=FACE_OUTER_BOUND('',#3626,.T.);
#2510=FACE_OUTER_BOUND('',#3628,.T.);
#2511=FACE_OUTER_BOUND('',#3629,.T.);
#2512=FACE_OUTER_BOUND('',#3630,.T.);
#2513=FACE_OUTER_BOUND('',#3631,.T.);
#2514=FACE_OUTER_BOUND('',#3632,.T.);
#2515=FACE_OUTER_BOUND('',#3633,.T.);
#2516=FACE_OUTER_BOUND('',#3638,.T.);
#2517=FACE_OUTER_BOUND('',#3643,.T.);
#2518=FACE_OUTER_BOUND('',#3644,.T.);
#2519=FACE_OUTER_BOUND('',#3645,.T.);
#2520=FACE_OUTER_BOUND('',#3646,.T.);
#2521=FACE_OUTER_BOUND('',#3647,.T.);
#2522=FACE_OUTER_BOUND('',#3649,.T.);
#2523=FACE_OUTER_BOUND('',#3650,.T.);
#2524=FACE_OUTER_BOUND('',#3651,.T.);
#2525=FACE_OUTER_BOUND('',#3653,.T.);
#2526=FACE_OUTER_BOUND('',#3655,.T.);
#2527=FACE_OUTER_BOUND('',#3656,.T.);
#2528=FACE_OUTER_BOUND('',#3657,.T.);
#2529=FACE_OUTER_BOUND('',#3659,.T.);
#2530=FACE_OUTER_BOUND('',#3661,.T.);
#2531=FACE_OUTER_BOUND('',#3662,.T.);
#2532=FACE_OUTER_BOUND('',#3663,.T.);
#2533=FACE_OUTER_BOUND('',#3665,.T.);
#2534=FACE_OUTER_BOUND('',#3667,.T.);
#2535=FACE_OUTER_BOUND('',#3668,.T.);
#2536=FACE_OUTER_BOUND('',#3669,.T.);
#2537=FACE_OUTER_BOUND('',#3670,.T.);
#2538=FACE_OUTER_BOUND('',#3671,.T.);
#2539=FACE_OUTER_BOUND('',#3673,.T.);
#2540=FACE_OUTER_BOUND('',#3674,.T.);
#2541=FACE_OUTER_BOUND('',#3675,.T.);
#2542=FACE_OUTER_BOUND('',#3676,.T.);
#2543=FACE_OUTER_BOUND('',#3677,.T.);
#2544=FACE_OUTER_BOUND('',#3678,.T.);
#2545=FACE_OUTER_BOUND('',#3679,.T.);
#2546=FACE_OUTER_BOUND('',#3680,.T.);
#2547=FACE_OUTER_BOUND('',#3681,.T.);
#2548=FACE_OUTER_BOUND('',#3682,.T.);
#2549=FACE_OUTER_BOUND('',#3683,.T.);
#2550=FACE_OUTER_BOUND('',#3684,.T.);
#2551=FACE_OUTER_BOUND('',#3685,.T.);
#2552=FACE_OUTER_BOUND('',#3686,.T.);
#2553=FACE_OUTER_BOUND('',#3687,.T.);
#2554=FACE_OUTER_BOUND('',#3688,.T.);
#2555=FACE_OUTER_BOUND('',#3689,.T.);
#2556=FACE_OUTER_BOUND('',#3693,.T.);
#2557=FACE_OUTER_BOUND('',#3694,.T.);
#2558=FACE_OUTER_BOUND('',#3698,.T.);
#2559=FACE_OUTER_BOUND('',#3699,.T.);
#2560=FACE_OUTER_BOUND('',#3700,.T.);
#2561=FACE_OUTER_BOUND('',#3701,.T.);
#2562=FACE_OUTER_BOUND('',#3702,.T.);
#2563=FACE_OUTER_BOUND('',#3703,.T.);
#2564=FACE_OUTER_BOUND('',#3704,.T.);
#2565=FACE_OUTER_BOUND('',#3705,.T.);
#2566=FACE_OUTER_BOUND('',#3706,.T.);
#2567=FACE_OUTER_BOUND('',#3707,.T.);
#2568=FACE_OUTER_BOUND('',#3711,.T.);
#2569=FACE_OUTER_BOUND('',#3715,.T.);
#2570=FACE_OUTER_BOUND('',#3716,.T.);
#2571=FACE_OUTER_BOUND('',#3717,.T.);
#2572=FACE_OUTER_BOUND('',#3718,.T.);
#2573=FACE_OUTER_BOUND('',#3719,.T.);
#2574=FACE_OUTER_BOUND('',#3720,.T.);
#2575=FACE_OUTER_BOUND('',#3721,.T.);
#2576=FACE_OUTER_BOUND('',#3722,.T.);
#2577=FACE_OUTER_BOUND('',#3726,.T.);
#2578=FACE_OUTER_BOUND('',#3730,.T.);
#2579=FACE_OUTER_BOUND('',#3731,.T.);
#2580=FACE_OUTER_BOUND('',#3733,.T.);
#2581=FACE_OUTER_BOUND('',#3734,.T.);
#2582=FACE_OUTER_BOUND('',#3736,.T.);
#2583=FACE_OUTER_BOUND('',#3737,.T.);
#2584=FACE_OUTER_BOUND('',#3738,.T.);
#2585=FACE_OUTER_BOUND('',#3739,.T.);
#2586=FACE_OUTER_BOUND('',#3740,.T.);
#2587=FACE_OUTER_BOUND('',#3741,.T.);
#2588=FACE_OUTER_BOUND('',#3743,.T.);
#2589=FACE_OUTER_BOUND('',#3744,.T.);
#2590=FACE_OUTER_BOUND('',#3745,.T.);
#2591=FACE_OUTER_BOUND('',#3746,.T.);
#2592=FACE_OUTER_BOUND('',#3748,.T.);
#2593=FACE_OUTER_BOUND('',#3749,.T.);
#2594=FACE_OUTER_BOUND('',#3750,.T.);
#2595=FACE_OUTER_BOUND('',#3752,.T.);
#2596=FACE_OUTER_BOUND('',#3754,.T.);
#2597=FACE_OUTER_BOUND('',#3755,.T.);
#2598=FACE_OUTER_BOUND('',#3756,.T.);
#2599=FACE_OUTER_BOUND('',#3758,.T.);
#2600=FACE_OUTER_BOUND('',#3760,.T.);
#2601=FACE_OUTER_BOUND('',#3761,.T.);
#2602=FACE_OUTER_BOUND('',#3762,.T.);
#2603=FACE_OUTER_BOUND('',#3763,.T.);
#2604=FACE_OUTER_BOUND('',#3764,.T.);
#2605=FACE_OUTER_BOUND('',#3765,.T.);
#2606=FACE_OUTER_BOUND('',#3767,.T.);
#2607=FACE_OUTER_BOUND('',#3768,.T.);
#2608=FACE_OUTER_BOUND('',#3770,.T.);
#2609=FACE_OUTER_BOUND('',#3771,.T.);
#2610=FACE_OUTER_BOUND('',#3773,.T.);
#2611=FACE_OUTER_BOUND('',#3774,.T.);
#2612=FACE_OUTER_BOUND('',#3776,.T.);
#2613=FACE_OUTER_BOUND('',#3777,.T.);
#2614=FACE_OUTER_BOUND('',#3779,.T.);
#2615=FACE_OUTER_BOUND('',#3780,.T.);
#2616=FACE_OUTER_BOUND('',#3782,.T.);
#2617=FACE_OUTER_BOUND('',#3784,.T.);
#2618=FACE_OUTER_BOUND('',#3785,.T.);
#2619=FACE_OUTER_BOUND('',#3786,.T.);
#2620=FACE_OUTER_BOUND('',#3787,.T.);
#2621=FACE_OUTER_BOUND('',#3788,.T.);
#2622=FACE_OUTER_BOUND('',#3790,.T.);
#2623=FACE_OUTER_BOUND('',#3792,.T.);
#2624=FACE_OUTER_BOUND('',#3794,.T.);
#2625=FACE_OUTER_BOUND('',#3796,.T.);
#2626=FACE_OUTER_BOUND('',#3797,.T.);
#2627=FACE_OUTER_BOUND('',#3798,.T.);
#2628=FACE_OUTER_BOUND('',#3799,.T.);
#2629=FACE_OUTER_BOUND('',#3800,.T.);
#2630=FACE_OUTER_BOUND('',#3801,.T.);
#2631=FACE_OUTER_BOUND('',#3802,.T.);
#2632=FACE_OUTER_BOUND('',#3803,.T.);
#2633=FACE_OUTER_BOUND('',#3804,.T.);
#2634=FACE_OUTER_BOUND('',#3805,.T.);
#2635=FACE_OUTER_BOUND('',#3806,.T.);
#2636=FACE_OUTER_BOUND('',#3807,.T.);
#2637=FACE_OUTER_BOUND('',#3808,.T.);
#2638=FACE_OUTER_BOUND('',#3809,.T.);
#2639=FACE_OUTER_BOUND('',#3811,.T.);
#2640=FACE_OUTER_BOUND('',#3812,.T.);
#2641=FACE_OUTER_BOUND('',#3813,.T.);
#2642=FACE_OUTER_BOUND('',#3814,.T.);
#2643=FACE_OUTER_BOUND('',#3815,.T.);
#2644=FACE_OUTER_BOUND('',#3818,.T.);
#2645=FACE_OUTER_BOUND('',#3819,.T.);
#2646=FACE_OUTER_BOUND('',#3820,.T.);
#2647=FACE_OUTER_BOUND('',#3821,.T.);
#2648=FACE_OUTER_BOUND('',#3822,.T.);
#2649=FACE_OUTER_BOUND('',#3825,.T.);
#2650=FACE_OUTER_BOUND('',#3826,.T.);
#2651=FACE_OUTER_BOUND('',#3827,.T.);
#2652=FACE_OUTER_BOUND('',#3828,.T.);
#2653=FACE_OUTER_BOUND('',#3829,.T.);
#2654=FACE_OUTER_BOUND('',#3830,.T.);
#2655=FACE_OUTER_BOUND('',#3832,.T.);
#2656=FACE_OUTER_BOUND('',#3834,.T.);
#2657=FACE_OUTER_BOUND('',#3835,.T.);
#2658=FACE_OUTER_BOUND('',#3836,.T.);
#2659=FACE_OUTER_BOUND('',#3838,.T.);
#2660=FACE_OUTER_BOUND('',#3840,.T.);
#2661=FACE_OUTER_BOUND('',#3841,.T.);
#2662=FACE_OUTER_BOUND('',#3842,.T.);
#2663=FACE_OUTER_BOUND('',#3844,.T.);
#2664=FACE_OUTER_BOUND('',#3846,.T.);
#2665=FACE_OUTER_BOUND('',#3847,.T.);
#2666=FACE_OUTER_BOUND('',#3848,.T.);
#2667=EDGE_LOOP('',(#8373,#8374,#8375,#8376));
#2668=EDGE_LOOP('',(#8377,#8378,#8379,#8380));
#2669=EDGE_LOOP('',(#8381,#8382,#8383,#8384));
#2670=EDGE_LOOP('',(#8385,#8386,#8387,#8388));
#2671=EDGE_LOOP('',(#8389,#8390,#8391,#8392));
#2672=EDGE_LOOP('',(#8393,#8394,#8395,#8396));
#2673=EDGE_LOOP('',(#8397,#8398,#8399,#8400));
#2674=EDGE_LOOP('',(#8401,#8402,#8403,#8404));
#2675=EDGE_LOOP('',(#8405,#8406,#8407,#8408));
#2676=EDGE_LOOP('',(#8409,#8410,#8411,#8412));
#2677=EDGE_LOOP('',(#8413,#8414,#8415,#8416));
#2678=EDGE_LOOP('',(#8417,#8418,#8419,#8420));
#2679=EDGE_LOOP('',(#8421,#8422,#8423,#8424));
#2680=EDGE_LOOP('',(#8425,#8426,#8427,#8428));
#2681=EDGE_LOOP('',(#8429,#8430,#8431,#8432));
#2682=EDGE_LOOP('',(#8433,#8434,#8435,#8436));
#2683=EDGE_LOOP('',(#8437,#8438,#8439,#8440));
#2684=EDGE_LOOP('',(#8441));
#2685=EDGE_LOOP('',(#8442));
#2686=EDGE_LOOP('',(#8443));
#2687=EDGE_LOOP('',(#8444));
#2688=EDGE_LOOP('',(#8445));
#2689=EDGE_LOOP('',(#8446));
#2690=EDGE_LOOP('',(#8447));
#2691=EDGE_LOOP('',(#8448));
#2692=EDGE_LOOP('',(#8449));
#2693=EDGE_LOOP('',(#8450));
#2694=EDGE_LOOP('',(#8451));
#2695=EDGE_LOOP('',(#8452));
#2696=EDGE_LOOP('',(#8453,#8454,#8455,#8456));
#2697=EDGE_LOOP('',(#8457));
#2698=EDGE_LOOP('',(#8458));
#2699=EDGE_LOOP('',(#8459));
#2700=EDGE_LOOP('',(#8460));
#2701=EDGE_LOOP('',(#8461));
#2702=EDGE_LOOP('',(#8462));
#2703=EDGE_LOOP('',(#8463));
#2704=EDGE_LOOP('',(#8464));
#2705=EDGE_LOOP('',(#8465));
#2706=EDGE_LOOP('',(#8466));
#2707=EDGE_LOOP('',(#8467));
#2708=EDGE_LOOP('',(#8468));
#2709=EDGE_LOOP('',(#8469,#8470,#8471,#8472));
#2710=EDGE_LOOP('',(#8473,#8474,#8475,#8476));
#2711=EDGE_LOOP('',(#8477,#8478,#8479,#8480));
#2712=EDGE_LOOP('',(#8481,#8482,#8483,#8484));
#2713=EDGE_LOOP('',(#8485,#8486,#8487,#8488));
#2714=EDGE_LOOP('',(#8489,#8490,#8491,#8492));
#2715=EDGE_LOOP('',(#8493,#8494,#8495,#8496));
#2716=EDGE_LOOP('',(#8497,#8498,#8499,#8500));
#2717=EDGE_LOOP('',(#8501,#8502,#8503,#8504));
#2718=EDGE_LOOP('',(#8505,#8506,#8507,#8508));
#2719=EDGE_LOOP('',(#8509,#8510,#8511,#8512));
#2720=EDGE_LOOP('',(#8513,#8514,#8515,#8516));
#2721=EDGE_LOOP('',(#8517,#8518,#8519,#8520));
#2722=EDGE_LOOP('',(#8521,#8522,#8523,#8524));
#2723=EDGE_LOOP('',(#8525,#8526,#8527,#8528));
#2724=EDGE_LOOP('',(#8529,#8530,#8531,#8532));
#2725=EDGE_LOOP('',(#8533,#8534,#8535,#8536));
#2726=EDGE_LOOP('',(#8537,#8538,#8539,#8540));
#2727=EDGE_LOOP('',(#8541,#8542,#8543,#8544));
#2728=EDGE_LOOP('',(#8545,#8546,#8547,#8548));
#2729=EDGE_LOOP('',(#8549,#8550,#8551,#8552,#8553,#8554,#8555,#8556));
#2730=EDGE_LOOP('',(#8557));
#2731=EDGE_LOOP('',(#8558));
#2732=EDGE_LOOP('',(#8559));
#2733=EDGE_LOOP('',(#8560));
#2734=EDGE_LOOP('',(#8561,#8562,#8563,#8564));
#2735=EDGE_LOOP('',(#8565,#8566,#8567,#8568));
#2736=EDGE_LOOP('',(#8569,#8570,#8571,#8572));
#2737=EDGE_LOOP('',(#8573,#8574,#8575,#8576,#8577,#8578,#8579,#8580));
#2738=EDGE_LOOP('',(#8581));
#2739=EDGE_LOOP('',(#8582));
#2740=EDGE_LOOP('',(#8583));
#2741=EDGE_LOOP('',(#8584));
#2742=EDGE_LOOP('',(#8585,#8586,#8587,#8588));
#2743=EDGE_LOOP('',(#8589,#8590,#8591,#8592));
#2744=EDGE_LOOP('',(#8593));
#2745=EDGE_LOOP('',(#8594));
#2746=EDGE_LOOP('',(#8595));
#2747=EDGE_LOOP('',(#8596));
#2748=EDGE_LOOP('',(#8597,#8598,#8599,#8600));
#2749=EDGE_LOOP('',(#8601,#8602,#8603,#8604));
#2750=EDGE_LOOP('',(#8605,#8606,#8607,#8608));
#2751=EDGE_LOOP('',(#8609));
#2752=EDGE_LOOP('',(#8610));
#2753=EDGE_LOOP('',(#8611));
#2754=EDGE_LOOP('',(#8612));
#2755=EDGE_LOOP('',(#8613,#8614,#8615,#8616));
#2756=EDGE_LOOP('',(#8617,#8618,#8619,#8620));
#2757=EDGE_LOOP('',(#8621,#8622,#8623,#8624));
#2758=EDGE_LOOP('',(#8625,#8626,#8627,#8628));
#2759=EDGE_LOOP('',(#8629,#8630,#8631,#8632));
#2760=EDGE_LOOP('',(#8633,#8634,#8635,#8636));
#2761=EDGE_LOOP('',(#8637,#8638,#8639,#8640));
#2762=EDGE_LOOP('',(#8641,#8642,#8643,#8644));
#2763=EDGE_LOOP('',(#8645,#8646,#8647,#8648,#8649,#8650,#8651,#8652));
#2764=EDGE_LOOP('',(#8653));
#2765=EDGE_LOOP('',(#8654));
#2766=EDGE_LOOP('',(#8655));
#2767=EDGE_LOOP('',(#8656));
#2768=EDGE_LOOP('',(#8657,#8658,#8659,#8660));
#2769=EDGE_LOOP('',(#8661,#8662,#8663,#8664));
#2770=EDGE_LOOP('',(#8665,#8666,#8667,#8668));
#2771=EDGE_LOOP('',(#8669,#8670,#8671,#8672,#8673,#8674,#8675,#8676));
#2772=EDGE_LOOP('',(#8677));
#2773=EDGE_LOOP('',(#8678));
#2774=EDGE_LOOP('',(#8679));
#2775=EDGE_LOOP('',(#8680));
#2776=EDGE_LOOP('',(#8681,#8682,#8683,#8684));
#2777=EDGE_LOOP('',(#8685,#8686,#8687,#8688));
#2778=EDGE_LOOP('',(#8689));
#2779=EDGE_LOOP('',(#8690));
#2780=EDGE_LOOP('',(#8691));
#2781=EDGE_LOOP('',(#8692));
#2782=EDGE_LOOP('',(#8693,#8694,#8695,#8696));
#2783=EDGE_LOOP('',(#8697,#8698,#8699,#8700));
#2784=EDGE_LOOP('',(#8701,#8702,#8703,#8704));
#2785=EDGE_LOOP('',(#8705));
#2786=EDGE_LOOP('',(#8706));
#2787=EDGE_LOOP('',(#8707));
#2788=EDGE_LOOP('',(#8708));
#2789=EDGE_LOOP('',(#8709,#8710,#8711,#8712));
#2790=EDGE_LOOP('',(#8713));
#2791=EDGE_LOOP('',(#8714,#8715,#8716,#8717));
#2792=EDGE_LOOP('',(#8718,#8719,#8720,#8721));
#2793=EDGE_LOOP('',(#8722,#8723,#8724,#8725));
#2794=EDGE_LOOP('',(#8726));
#2795=EDGE_LOOP('',(#8727));
#2796=EDGE_LOOP('',(#8728));
#2797=EDGE_LOOP('',(#8729));
#2798=EDGE_LOOP('',(#8730));
#2799=EDGE_LOOP('',(#8731));
#2800=EDGE_LOOP('',(#8732));
#2801=EDGE_LOOP('',(#8733));
#2802=EDGE_LOOP('',(#8734));
#2803=EDGE_LOOP('',(#8735));
#2804=EDGE_LOOP('',(#8736,#8737,#8738,#8739));
#2805=EDGE_LOOP('',(#8740,#8741,#8742,#8743));
#2806=EDGE_LOOP('',(#8744,#8745,#8746,#8747));
#2807=EDGE_LOOP('',(#8748));
#2808=EDGE_LOOP('',(#8749));
#2809=EDGE_LOOP('',(#8750));
#2810=EDGE_LOOP('',(#8751,#8752,#8753,#8754));
#2811=EDGE_LOOP('',(#8755,#8756,#8757,#8758));
#2812=EDGE_LOOP('',(#8759));
#2813=EDGE_LOOP('',(#8760));
#2814=EDGE_LOOP('',(#8761));
#2815=EDGE_LOOP('',(#8762));
#2816=EDGE_LOOP('',(#8763,#8764,#8765,#8766));
#2817=EDGE_LOOP('',(#8767,#8768,#8769,#8770));
#2818=EDGE_LOOP('',(#8771));
#2819=EDGE_LOOP('',(#8772));
#2820=EDGE_LOOP('',(#8773));
#2821=EDGE_LOOP('',(#8774));
#2822=EDGE_LOOP('',(#8775,#8776,#8777,#8778));
#2823=EDGE_LOOP('',(#8779,#8780,#8781,#8782));
#2824=EDGE_LOOP('',(#8783));
#2825=EDGE_LOOP('',(#8784));
#2826=EDGE_LOOP('',(#8785));
#2827=EDGE_LOOP('',(#8786));
#2828=EDGE_LOOP('',(#8787,#8788,#8789,#8790));
#2829=EDGE_LOOP('',(#8791));
#2830=EDGE_LOOP('',(#8792,#8793,#8794,#8795));
#2831=EDGE_LOOP('',(#8796,#8797,#8798,#8799));
#2832=EDGE_LOOP('',(#8800,#8801,#8802,#8803));
#2833=EDGE_LOOP('',(#8804));
#2834=EDGE_LOOP('',(#8805));
#2835=EDGE_LOOP('',(#8806));
#2836=EDGE_LOOP('',(#8807));
#2837=EDGE_LOOP('',(#8808));
#2838=EDGE_LOOP('',(#8809));
#2839=EDGE_LOOP('',(#8810));
#2840=EDGE_LOOP('',(#8811));
#2841=EDGE_LOOP('',(#8812));
#2842=EDGE_LOOP('',(#8813));
#2843=EDGE_LOOP('',(#8814,#8815,#8816,#8817));
#2844=EDGE_LOOP('',(#8818,#8819,#8820,#8821));
#2845=EDGE_LOOP('',(#8822,#8823,#8824,#8825));
#2846=EDGE_LOOP('',(#8826));
#2847=EDGE_LOOP('',(#8827));
#2848=EDGE_LOOP('',(#8828));
#2849=EDGE_LOOP('',(#8829,#8830,#8831,#8832));
#2850=EDGE_LOOP('',(#8833,#8834,#8835,#8836));
#2851=EDGE_LOOP('',(#8837));
#2852=EDGE_LOOP('',(#8838));
#2853=EDGE_LOOP('',(#8839));
#2854=EDGE_LOOP('',(#8840));
#2855=EDGE_LOOP('',(#8841,#8842,#8843,#8844));
#2856=EDGE_LOOP('',(#8845,#8846,#8847,#8848));
#2857=EDGE_LOOP('',(#8849));
#2858=EDGE_LOOP('',(#8850));
#2859=EDGE_LOOP('',(#8851));
#2860=EDGE_LOOP('',(#8852));
#2861=EDGE_LOOP('',(#8853,#8854,#8855,#8856));
#2862=EDGE_LOOP('',(#8857,#8858,#8859,#8860));
#2863=EDGE_LOOP('',(#8861));
#2864=EDGE_LOOP('',(#8862));
#2865=EDGE_LOOP('',(#8863));
#2866=EDGE_LOOP('',(#8864));
#2867=EDGE_LOOP('',(#8865,#8866,#8867,#8868));
#2868=EDGE_LOOP('',(#8869,#8870,#8871,#8872));
#2869=EDGE_LOOP('',(#8873,#8874,#8875,#8876));
#2870=EDGE_LOOP('',(#8877));
#2871=EDGE_LOOP('',(#8878,#8879,#8880,#8881,#8882,#8883));
#2872=EDGE_LOOP('',(#8884));
#2873=EDGE_LOOP('',(#8885));
#2874=EDGE_LOOP('',(#8886));
#2875=EDGE_LOOP('',(#8887));
#2876=EDGE_LOOP('',(#8888,#8889,#8890,#8891));
#2877=EDGE_LOOP('',(#8892));
#2878=EDGE_LOOP('',(#8893));
#2879=EDGE_LOOP('',(#8894,#8895,#8896,#8897));
#2880=EDGE_LOOP('',(#8898,#8899,#8900,#8901));
#2881=EDGE_LOOP('',(#8902));
#2882=EDGE_LOOP('',(#8903));
#2883=EDGE_LOOP('',(#8904,#8905,#8906,#8907));
#2884=EDGE_LOOP('',(#8908,#8909,#8910,#8911));
#2885=EDGE_LOOP('',(#8912,#8913,#8914,#8915));
#2886=EDGE_LOOP('',(#8916,#8917,#8918,#8919));
#2887=EDGE_LOOP('',(#8920,#8921,#8922,#8923));
#2888=EDGE_LOOP('',(#8924,#8925,#8926,#8927));
#2889=EDGE_LOOP('',(#8928,#8929,#8930,#8931,#8932,#8933));
#2890=EDGE_LOOP('',(#8934));
#2891=EDGE_LOOP('',(#8935));
#2892=EDGE_LOOP('',(#8936));
#2893=EDGE_LOOP('',(#8937));
#2894=EDGE_LOOP('',(#8938,#8939,#8940,#8941));
#2895=EDGE_LOOP('',(#8942));
#2896=EDGE_LOOP('',(#8943,#8944,#8945,#8946));
#2897=EDGE_LOOP('',(#8947));
#2898=EDGE_LOOP('',(#8948));
#2899=EDGE_LOOP('',(#8949,#8950,#8951,#8952));
#2900=EDGE_LOOP('',(#8953,#8954,#8955,#8956));
#2901=EDGE_LOOP('',(#8957,#8958,#8959,#8960));
#2902=EDGE_LOOP('',(#8961,#8962,#8963,#8964));
#2903=EDGE_LOOP('',(#8965,#8966,#8967,#8968));
#2904=EDGE_LOOP('',(#8969));
#2905=EDGE_LOOP('',(#8970));
#2906=EDGE_LOOP('',(#8971));
#2907=EDGE_LOOP('',(#8972,#8973,#8974,#8975));
#2908=EDGE_LOOP('',(#8976,#8977,#8978,#8979));
#2909=EDGE_LOOP('',(#8980,#8981,#8982,#8983));
#2910=EDGE_LOOP('',(#8984,#8985,#8986,#8987));
#2911=EDGE_LOOP('',(#8988));
#2912=EDGE_LOOP('',(#8989));
#2913=EDGE_LOOP('',(#8990));
#2914=EDGE_LOOP('',(#8991));
#2915=EDGE_LOOP('',(#8992));
#2916=EDGE_LOOP('',(#8993,#8994,#8995,#8996));
#2917=EDGE_LOOP('',(#8997));
#2918=EDGE_LOOP('',(#8998,#8999,#9000,#9001));
#2919=EDGE_LOOP('',(#9002));
#2920=EDGE_LOOP('',(#9003));
#2921=EDGE_LOOP('',(#9004));
#2922=EDGE_LOOP('',(#9005,#9006,#9007,#9008));
#2923=EDGE_LOOP('',(#9009));
#2924=EDGE_LOOP('',(#9010,#9011,#9012,#9013));
#2925=EDGE_LOOP('',(#9014));
#2926=EDGE_LOOP('',(#9015,#9016,#9017,#9018));
#2927=EDGE_LOOP('',(#9019,#9020,#9021,#9022));
#2928=EDGE_LOOP('',(#9023,#9024,#9025,#9026));
#2929=EDGE_LOOP('',(#9027,#9028,#9029,#9030));
#2930=EDGE_LOOP('',(#9031,#9032,#9033,#9034));
#2931=EDGE_LOOP('',(#9035));
#2932=EDGE_LOOP('',(#9036));
#2933=EDGE_LOOP('',(#9037));
#2934=EDGE_LOOP('',(#9038,#9039,#9040,#9041));
#2935=EDGE_LOOP('',(#9042,#9043,#9044,#9045));
#2936=EDGE_LOOP('',(#9046,#9047,#9048,#9049));
#2937=EDGE_LOOP('',(#9050,#9051,#9052,#9053));
#2938=EDGE_LOOP('',(#9054));
#2939=EDGE_LOOP('',(#9055));
#2940=EDGE_LOOP('',(#9056));
#2941=EDGE_LOOP('',(#9057));
#2942=EDGE_LOOP('',(#9058));
#2943=EDGE_LOOP('',(#9059,#9060,#9061,#9062));
#2944=EDGE_LOOP('',(#9063));
#2945=EDGE_LOOP('',(#9064,#9065,#9066,#9067));
#2946=EDGE_LOOP('',(#9068));
#2947=EDGE_LOOP('',(#9069));
#2948=EDGE_LOOP('',(#9070));
#2949=EDGE_LOOP('',(#9071,#9072,#9073,#9074));
#2950=EDGE_LOOP('',(#9075));
#2951=EDGE_LOOP('',(#9076,#9077,#9078,#9079));
#2952=EDGE_LOOP('',(#9080));
#2953=EDGE_LOOP('',(#9081,#9082,#9083,#9084));
#2954=EDGE_LOOP('',(#9085,#9086,#9087,#9088));
#2955=EDGE_LOOP('',(#9089,#9090,#9091,#9092));
#2956=EDGE_LOOP('',(#9093));
#2957=EDGE_LOOP('',(#9094,#9095,#9096,#9097,#9098,#9099));
#2958=EDGE_LOOP('',(#9100));
#2959=EDGE_LOOP('',(#9101));
#2960=EDGE_LOOP('',(#9102));
#2961=EDGE_LOOP('',(#9103));
#2962=EDGE_LOOP('',(#9104,#9105,#9106,#9107));
#2963=EDGE_LOOP('',(#9108));
#2964=EDGE_LOOP('',(#9109));
#2965=EDGE_LOOP('',(#9110,#9111,#9112,#9113));
#2966=EDGE_LOOP('',(#9114,#9115,#9116,#9117));
#2967=EDGE_LOOP('',(#9118));
#2968=EDGE_LOOP('',(#9119));
#2969=EDGE_LOOP('',(#9120,#9121,#9122,#9123));
#2970=EDGE_LOOP('',(#9124,#9125,#9126,#9127));
#2971=EDGE_LOOP('',(#9128,#9129,#9130,#9131));
#2972=EDGE_LOOP('',(#9132,#9133,#9134,#9135));
#2973=EDGE_LOOP('',(#9136,#9137,#9138,#9139));
#2974=EDGE_LOOP('',(#9140,#9141,#9142,#9143));
#2975=EDGE_LOOP('',(#9144,#9145,#9146,#9147,#9148,#9149));
#2976=EDGE_LOOP('',(#9150));
#2977=EDGE_LOOP('',(#9151));
#2978=EDGE_LOOP('',(#9152));
#2979=EDGE_LOOP('',(#9153));
#2980=EDGE_LOOP('',(#9154,#9155,#9156,#9157));
#2981=EDGE_LOOP('',(#9158));
#2982=EDGE_LOOP('',(#9159,#9160,#9161,#9162));
#2983=EDGE_LOOP('',(#9163));
#2984=EDGE_LOOP('',(#9164));
#2985=EDGE_LOOP('',(#9165,#9166,#9167,#9168));
#2986=EDGE_LOOP('',(#9169,#9170,#9171,#9172));
#2987=EDGE_LOOP('',(#9173,#9174,#9175,#9176));
#2988=EDGE_LOOP('',(#9177,#9178,#9179,#9180));
#2989=EDGE_LOOP('',(#9181,#9182,#9183,#9184));
#2990=EDGE_LOOP('',(#9185));
#2991=EDGE_LOOP('',(#9186));
#2992=EDGE_LOOP('',(#9187));
#2993=EDGE_LOOP('',(#9188,#9189,#9190,#9191));
#2994=EDGE_LOOP('',(#9192,#9193,#9194,#9195));
#2995=EDGE_LOOP('',(#9196,#9197,#9198,#9199));
#2996=EDGE_LOOP('',(#9200,#9201,#9202,#9203));
#2997=EDGE_LOOP('',(#9204));
#2998=EDGE_LOOP('',(#9205));
#2999=EDGE_LOOP('',(#9206));
#3000=EDGE_LOOP('',(#9207));
#3001=EDGE_LOOP('',(#9208));
#3002=EDGE_LOOP('',(#9209,#9210,#9211,#9212));
#3003=EDGE_LOOP('',(#9213));
#3004=EDGE_LOOP('',(#9214,#9215,#9216,#9217));
#3005=EDGE_LOOP('',(#9218));
#3006=EDGE_LOOP('',(#9219));
#3007=EDGE_LOOP('',(#9220));
#3008=EDGE_LOOP('',(#9221,#9222,#9223,#9224));
#3009=EDGE_LOOP('',(#9225));
#3010=EDGE_LOOP('',(#9226,#9227,#9228,#9229));
#3011=EDGE_LOOP('',(#9230));
#3012=EDGE_LOOP('',(#9231,#9232,#9233,#9234));
#3013=EDGE_LOOP('',(#9235,#9236,#9237,#9238));
#3014=EDGE_LOOP('',(#9239,#9240,#9241,#9242));
#3015=EDGE_LOOP('',(#9243,#9244,#9245,#9246));
#3016=EDGE_LOOP('',(#9247,#9248,#9249,#9250));
#3017=EDGE_LOOP('',(#9251));
#3018=EDGE_LOOP('',(#9252));
#3019=EDGE_LOOP('',(#9253));
#3020=EDGE_LOOP('',(#9254,#9255,#9256,#9257));
#3021=EDGE_LOOP('',(#9258,#9259,#9260,#9261));
#3022=EDGE_LOOP('',(#9262,#9263,#9264,#9265));
#3023=EDGE_LOOP('',(#9266,#9267,#9268,#9269));
#3024=EDGE_LOOP('',(#9270));
#3025=EDGE_LOOP('',(#9271));
#3026=EDGE_LOOP('',(#9272));
#3027=EDGE_LOOP('',(#9273));
#3028=EDGE_LOOP('',(#9274));
#3029=EDGE_LOOP('',(#9275,#9276,#9277,#9278));
#3030=EDGE_LOOP('',(#9279));
#3031=EDGE_LOOP('',(#9280,#9281,#9282,#9283));
#3032=EDGE_LOOP('',(#9284));
#3033=EDGE_LOOP('',(#9285));
#3034=EDGE_LOOP('',(#9286));
#3035=EDGE_LOOP('',(#9287,#9288,#9289,#9290));
#3036=EDGE_LOOP('',(#9291));
#3037=EDGE_LOOP('',(#9292,#9293,#9294,#9295));
#3038=EDGE_LOOP('',(#9296));
#3039=EDGE_LOOP('',(#9297,#9298,#9299,#9300));
#3040=EDGE_LOOP('',(#9301));
#3041=EDGE_LOOP('',(#9302));
#3042=EDGE_LOOP('',(#9303,#9304,#9305,#9306));
#3043=EDGE_LOOP('',(#9307));
#3044=EDGE_LOOP('',(#9308));
#3045=EDGE_LOOP('',(#9309));
#3046=EDGE_LOOP('',(#9310,#9311,#9312,#9313));
#3047=EDGE_LOOP('',(#9314,#9315,#9316,#9317));
#3048=EDGE_LOOP('',(#9318,#9319,#9320,#9321));
#3049=EDGE_LOOP('',(#9322));
#3050=EDGE_LOOP('',(#9323));
#3051=EDGE_LOOP('',(#9324,#9325,#9326,#9327));
#3052=EDGE_LOOP('',(#9328,#9329,#9330,#9331));
#3053=EDGE_LOOP('',(#9332,#9333,#9334,#9335));
#3054=EDGE_LOOP('',(#9336));
#3055=EDGE_LOOP('',(#9337,#9338,#9339,#9340));
#3056=EDGE_LOOP('',(#9341,#9342,#9343,#9344));
#3057=EDGE_LOOP('',(#9345,#9346,#9347,#9348));
#3058=EDGE_LOOP('',(#9349,#9350,#9351,#9352));
#3059=EDGE_LOOP('',(#9353,#9354,#9355,#9356));
#3060=EDGE_LOOP('',(#9357,#9358,#9359,#9360));
#3061=EDGE_LOOP('',(#9361,#9362,#9363,#9364,#9365,#9366));
#3062=EDGE_LOOP('',(#9367,#9368,#9369,#9370,#9371,#9372));
#3063=EDGE_LOOP('',(#9373,#9374,#9375,#9376));
#3064=EDGE_LOOP('',(#9377,#9378,#9379,#9380));
#3065=EDGE_LOOP('',(#9381,#9382,#9383,#9384));
#3066=EDGE_LOOP('',(#9385,#9386,#9387,#9388));
#3067=EDGE_LOOP('',(#9389,#9390,#9391,#9392));
#3068=EDGE_LOOP('',(#9393,#9394,#9395,#9396));
#3069=EDGE_LOOP('',(#9397,#9398,#9399,#9400));
#3070=EDGE_LOOP('',(#9401));
#3071=EDGE_LOOP('',(#9402));
#3072=EDGE_LOOP('',(#9403));
#3073=EDGE_LOOP('',(#9404));
#3074=EDGE_LOOP('',(#9405));
#3075=EDGE_LOOP('',(#9406));
#3076=EDGE_LOOP('',(#9407));
#3077=EDGE_LOOP('',(#9408));
#3078=EDGE_LOOP('',(#9409));
#3079=EDGE_LOOP('',(#9410));
#3080=EDGE_LOOP('',(#9411,#9412,#9413,#9414));
#3081=EDGE_LOOP('',(#9415,#9416,#9417,#9418));
#3082=EDGE_LOOP('',(#9419,#9420,#9421,#9422));
#3083=EDGE_LOOP('',(#9423,#9424,#9425,#9426));
#3084=EDGE_LOOP('',(#9427,#9428,#9429,#9430));
#3085=EDGE_LOOP('',(#9431,#9432,#9433,#9434));
#3086=EDGE_LOOP('',(#9435,#9436,#9437,#9438));
#3087=EDGE_LOOP('',(#9439,#9440,#9441,#9442));
#3088=EDGE_LOOP('',(#9443,#9444,#9445,#9446));
#3089=EDGE_LOOP('',(#9447));
#3090=EDGE_LOOP('',(#9448));
#3091=EDGE_LOOP('',(#9449));
#3092=EDGE_LOOP('',(#9450));
#3093=EDGE_LOOP('',(#9451));
#3094=EDGE_LOOP('',(#9452));
#3095=EDGE_LOOP('',(#9453));
#3096=EDGE_LOOP('',(#9454));
#3097=EDGE_LOOP('',(#9455));
#3098=EDGE_LOOP('',(#9456));
#3099=EDGE_LOOP('',(#9457,#9458,#9459,#9460));
#3100=EDGE_LOOP('',(#9461,#9462,#9463,#9464));
#3101=EDGE_LOOP('',(#9465,#9466,#9467,#9468));
#3102=EDGE_LOOP('',(#9469,#9470,#9471,#9472));
#3103=EDGE_LOOP('',(#9473,#9474,#9475,#9476));
#3104=EDGE_LOOP('',(#9477,#9478,#9479,#9480));
#3105=EDGE_LOOP('',(#9481));
#3106=EDGE_LOOP('',(#9482));
#3107=EDGE_LOOP('',(#9483));
#3108=EDGE_LOOP('',(#9484));
#3109=EDGE_LOOP('',(#9485));
#3110=EDGE_LOOP('',(#9486));
#3111=EDGE_LOOP('',(#9487));
#3112=EDGE_LOOP('',(#9488));
#3113=EDGE_LOOP('',(#9489));
#3114=EDGE_LOOP('',(#9490));
#3115=EDGE_LOOP('',(#9491));
#3116=EDGE_LOOP('',(#9492));
#3117=EDGE_LOOP('',(#9493));
#3118=EDGE_LOOP('',(#9494));
#3119=EDGE_LOOP('',(#9495,#9496,#9497,#9498));
#3120=EDGE_LOOP('',(#9499));
#3121=EDGE_LOOP('',(#9500,#9501,#9502,#9503));
#3122=EDGE_LOOP('',(#9504));
#3123=EDGE_LOOP('',(#9505));
#3124=EDGE_LOOP('',(#9506));
#3125=EDGE_LOOP('',(#9507,#9508,#9509,#9510));
#3126=EDGE_LOOP('',(#9511));
#3127=EDGE_LOOP('',(#9512,#9513,#9514,#9515));
#3128=EDGE_LOOP('',(#9516));
#3129=EDGE_LOOP('',(#9517));
#3130=EDGE_LOOP('',(#9518));
#3131=EDGE_LOOP('',(#9519,#9520,#9521,#9522));
#3132=EDGE_LOOP('',(#9523));
#3133=EDGE_LOOP('',(#9524,#9525,#9526,#9527));
#3134=EDGE_LOOP('',(#9528));
#3135=EDGE_LOOP('',(#9529));
#3136=EDGE_LOOP('',(#9530));
#3137=EDGE_LOOP('',(#9531,#9532,#9533,#9534));
#3138=EDGE_LOOP('',(#9535));
#3139=EDGE_LOOP('',(#9536,#9537,#9538,#9539));
#3140=EDGE_LOOP('',(#9540));
#3141=EDGE_LOOP('',(#9541,#9542,#9543,#9544));
#3142=EDGE_LOOP('',(#9545,#9546,#9547,#9548));
#3143=EDGE_LOOP('',(#9549,#9550,#9551,#9552));
#3144=EDGE_LOOP('',(#9553,#9554,#9555,#9556));
#3145=EDGE_LOOP('',(#9557,#9558,#9559,#9560));
#3146=EDGE_LOOP('',(#9561,#9562,#9563,#9564));
#3147=EDGE_LOOP('',(#9565));
#3148=EDGE_LOOP('',(#9566));
#3149=EDGE_LOOP('',(#9567));
#3150=EDGE_LOOP('',(#9568));
#3151=EDGE_LOOP('',(#9569));
#3152=EDGE_LOOP('',(#9570));
#3153=EDGE_LOOP('',(#9571));
#3154=EDGE_LOOP('',(#9572));
#3155=EDGE_LOOP('',(#9573));
#3156=EDGE_LOOP('',(#9574));
#3157=EDGE_LOOP('',(#9575));
#3158=EDGE_LOOP('',(#9576));
#3159=EDGE_LOOP('',(#9577));
#3160=EDGE_LOOP('',(#9578));
#3161=EDGE_LOOP('',(#9579,#9580,#9581,#9582));
#3162=EDGE_LOOP('',(#9583));
#3163=EDGE_LOOP('',(#9584,#9585,#9586,#9587));
#3164=EDGE_LOOP('',(#9588));
#3165=EDGE_LOOP('',(#9589));
#3166=EDGE_LOOP('',(#9590));
#3167=EDGE_LOOP('',(#9591,#9592,#9593,#9594));
#3168=EDGE_LOOP('',(#9595));
#3169=EDGE_LOOP('',(#9596,#9597,#9598,#9599));
#3170=EDGE_LOOP('',(#9600));
#3171=EDGE_LOOP('',(#9601));
#3172=EDGE_LOOP('',(#9602));
#3173=EDGE_LOOP('',(#9603,#9604,#9605,#9606));
#3174=EDGE_LOOP('',(#9607));
#3175=EDGE_LOOP('',(#9608,#9609,#9610,#9611));
#3176=EDGE_LOOP('',(#9612));
#3177=EDGE_LOOP('',(#9613));
#3178=EDGE_LOOP('',(#9614));
#3179=EDGE_LOOP('',(#9615,#9616,#9617,#9618));
#3180=EDGE_LOOP('',(#9619));
#3181=EDGE_LOOP('',(#9620,#9621,#9622,#9623));
#3182=EDGE_LOOP('',(#9624));
#3183=EDGE_LOOP('',(#9625,#9626,#9627,#9628));
#3184=EDGE_LOOP('',(#9629,#9630,#9631,#9632));
#3185=EDGE_LOOP('',(#9633,#9634,#9635,#9636));
#3186=EDGE_LOOP('',(#9637,#9638,#9639,#9640));
#3187=EDGE_LOOP('',(#9641,#9642,#9643,#9644));
#3188=EDGE_LOOP('',(#9645,#9646,#9647,#9648));
#3189=EDGE_LOOP('',(#9649));
#3190=EDGE_LOOP('',(#9650));
#3191=EDGE_LOOP('',(#9651));
#3192=EDGE_LOOP('',(#9652));
#3193=EDGE_LOOP('',(#9653));
#3194=EDGE_LOOP('',(#9654));
#3195=EDGE_LOOP('',(#9655));
#3196=EDGE_LOOP('',(#9656));
#3197=EDGE_LOOP('',(#9657));
#3198=EDGE_LOOP('',(#9658));
#3199=EDGE_LOOP('',(#9659));
#3200=EDGE_LOOP('',(#9660));
#3201=EDGE_LOOP('',(#9661));
#3202=EDGE_LOOP('',(#9662));
#3203=EDGE_LOOP('',(#9663,#9664,#9665,#9666));
#3204=EDGE_LOOP('',(#9667));
#3205=EDGE_LOOP('',(#9668,#9669,#9670,#9671));
#3206=EDGE_LOOP('',(#9672));
#3207=EDGE_LOOP('',(#9673));
#3208=EDGE_LOOP('',(#9674));
#3209=EDGE_LOOP('',(#9675,#9676,#9677,#9678));
#3210=EDGE_LOOP('',(#9679));
#3211=EDGE_LOOP('',(#9680,#9681,#9682,#9683));
#3212=EDGE_LOOP('',(#9684));
#3213=EDGE_LOOP('',(#9685));
#3214=EDGE_LOOP('',(#9686));
#3215=EDGE_LOOP('',(#9687,#9688,#9689,#9690));
#3216=EDGE_LOOP('',(#9691));
#3217=EDGE_LOOP('',(#9692,#9693,#9694,#9695));
#3218=EDGE_LOOP('',(#9696));
#3219=EDGE_LOOP('',(#9697));
#3220=EDGE_LOOP('',(#9698));
#3221=EDGE_LOOP('',(#9699,#9700,#9701,#9702));
#3222=EDGE_LOOP('',(#9703));
#3223=EDGE_LOOP('',(#9704,#9705,#9706,#9707));
#3224=EDGE_LOOP('',(#9708));
#3225=EDGE_LOOP('',(#9709,#9710,#9711,#9712));
#3226=EDGE_LOOP('',(#9713,#9714,#9715,#9716));
#3227=EDGE_LOOP('',(#9717,#9718,#9719,#9720));
#3228=EDGE_LOOP('',(#9721,#9722,#9723,#9724));
#3229=EDGE_LOOP('',(#9725,#9726,#9727,#9728));
#3230=EDGE_LOOP('',(#9729,#9730,#9731,#9732));
#3231=EDGE_LOOP('',(#9733));
#3232=EDGE_LOOP('',(#9734));
#3233=EDGE_LOOP('',(#9735));
#3234=EDGE_LOOP('',(#9736));
#3235=EDGE_LOOP('',(#9737));
#3236=EDGE_LOOP('',(#9738));
#3237=EDGE_LOOP('',(#9739));
#3238=EDGE_LOOP('',(#9740));
#3239=EDGE_LOOP('',(#9741));
#3240=EDGE_LOOP('',(#9742));
#3241=EDGE_LOOP('',(#9743));
#3242=EDGE_LOOP('',(#9744));
#3243=EDGE_LOOP('',(#9745));
#3244=EDGE_LOOP('',(#9746));
#3245=EDGE_LOOP('',(#9747,#9748,#9749,#9750));
#3246=EDGE_LOOP('',(#9751));
#3247=EDGE_LOOP('',(#9752,#9753,#9754,#9755));
#3248=EDGE_LOOP('',(#9756));
#3249=EDGE_LOOP('',(#9757));
#3250=EDGE_LOOP('',(#9758));
#3251=EDGE_LOOP('',(#9759,#9760,#9761,#9762));
#3252=EDGE_LOOP('',(#9763));
#3253=EDGE_LOOP('',(#9764,#9765,#9766,#9767));
#3254=EDGE_LOOP('',(#9768));
#3255=EDGE_LOOP('',(#9769));
#3256=EDGE_LOOP('',(#9770));
#3257=EDGE_LOOP('',(#9771,#9772,#9773,#9774));
#3258=EDGE_LOOP('',(#9775));
#3259=EDGE_LOOP('',(#9776,#9777,#9778,#9779));
#3260=EDGE_LOOP('',(#9780));
#3261=EDGE_LOOP('',(#9781));
#3262=EDGE_LOOP('',(#9782));
#3263=EDGE_LOOP('',(#9783,#9784,#9785,#9786));
#3264=EDGE_LOOP('',(#9787));
#3265=EDGE_LOOP('',(#9788,#9789,#9790,#9791));
#3266=EDGE_LOOP('',(#9792));
#3267=EDGE_LOOP('',(#9793,#9794,#9795,#9796));
#3268=EDGE_LOOP('',(#9797,#9798,#9799,#9800));
#3269=EDGE_LOOP('',(#9801,#9802,#9803,#9804));
#3270=EDGE_LOOP('',(#9805,#9806,#9807,#9808));
#3271=EDGE_LOOP('',(#9809,#9810,#9811,#9812));
#3272=EDGE_LOOP('',(#9813,#9814,#9815,#9816));
#3273=EDGE_LOOP('',(#9817,#9818,#9819,#9820));
#3274=EDGE_LOOP('',(#9821,#9822,#9823,#9824));
#3275=EDGE_LOOP('',(#9825));
#3276=EDGE_LOOP('',(#9826));
#3277=EDGE_LOOP('',(#9827));
#3278=EDGE_LOOP('',(#9828));
#3279=EDGE_LOOP('',(#9829));
#3280=EDGE_LOOP('',(#9830));
#3281=EDGE_LOOP('',(#9831));
#3282=EDGE_LOOP('',(#9832));
#3283=EDGE_LOOP('',(#9833));
#3284=EDGE_LOOP('',(#9834));
#3285=EDGE_LOOP('',(#9835,#9836,#9837,#9838));
#3286=EDGE_LOOP('',(#9839,#9840,#9841,#9842));
#3287=EDGE_LOOP('',(#9843,#9844,#9845,#9846));
#3288=EDGE_LOOP('',(#9847,#9848,#9849,#9850));
#3289=EDGE_LOOP('',(#9851,#9852,#9853,#9854));
#3290=EDGE_LOOP('',(#9855,#9856,#9857,#9858));
#3291=EDGE_LOOP('',(#9859,#9860,#9861,#9862));
#3292=EDGE_LOOP('',(#9863,#9864,#9865,#9866));
#3293=EDGE_LOOP('',(#9867));
#3294=EDGE_LOOP('',(#9868));
#3295=EDGE_LOOP('',(#9869));
#3296=EDGE_LOOP('',(#9870));
#3297=EDGE_LOOP('',(#9871));
#3298=EDGE_LOOP('',(#9872));
#3299=EDGE_LOOP('',(#9873));
#3300=EDGE_LOOP('',(#9874));
#3301=EDGE_LOOP('',(#9875));
#3302=EDGE_LOOP('',(#9876));
#3303=EDGE_LOOP('',(#9877,#9878,#9879,#9880));
#3304=EDGE_LOOP('',(#9881,#9882,#9883,#9884));
#3305=EDGE_LOOP('',(#9885,#9886,#9887,#9888));
#3306=EDGE_LOOP('',(#9889,#9890,#9891,#9892));
#3307=EDGE_LOOP('',(#9893,#9894,#9895,#9896));
#3308=EDGE_LOOP('',(#9897,#9898,#9899,#9900));
#3309=EDGE_LOOP('',(#9901));
#3310=EDGE_LOOP('',(#9902));
#3311=EDGE_LOOP('',(#9903));
#3312=EDGE_LOOP('',(#9904));
#3313=EDGE_LOOP('',(#9905));
#3314=EDGE_LOOP('',(#9906));
#3315=EDGE_LOOP('',(#9907));
#3316=EDGE_LOOP('',(#9908));
#3317=EDGE_LOOP('',(#9909));
#3318=EDGE_LOOP('',(#9910));
#3319=EDGE_LOOP('',(#9911));
#3320=EDGE_LOOP('',(#9912));
#3321=EDGE_LOOP('',(#9913));
#3322=EDGE_LOOP('',(#9914));
#3323=EDGE_LOOP('',(#9915,#9916,#9917,#9918));
#3324=EDGE_LOOP('',(#9919));
#3325=EDGE_LOOP('',(#9920,#9921,#9922,#9923));
#3326=EDGE_LOOP('',(#9924));
#3327=EDGE_LOOP('',(#9925));
#3328=EDGE_LOOP('',(#9926));
#3329=EDGE_LOOP('',(#9927,#9928,#9929,#9930));
#3330=EDGE_LOOP('',(#9931));
#3331=EDGE_LOOP('',(#9932,#9933,#9934,#9935));
#3332=EDGE_LOOP('',(#9936));
#3333=EDGE_LOOP('',(#9937));
#3334=EDGE_LOOP('',(#9938));
#3335=EDGE_LOOP('',(#9939,#9940,#9941,#9942));
#3336=EDGE_LOOP('',(#9943));
#3337=EDGE_LOOP('',(#9944,#9945,#9946,#9947));
#3338=EDGE_LOOP('',(#9948));
#3339=EDGE_LOOP('',(#9949));
#3340=EDGE_LOOP('',(#9950));
#3341=EDGE_LOOP('',(#9951,#9952,#9953,#9954));
#3342=EDGE_LOOP('',(#9955));
#3343=EDGE_LOOP('',(#9956,#9957,#9958,#9959));
#3344=EDGE_LOOP('',(#9960));
#3345=EDGE_LOOP('',(#9961,#9962,#9963,#9964));
#3346=EDGE_LOOP('',(#9965,#9966,#9967,#9968));
#3347=EDGE_LOOP('',(#9969,#9970,#9971,#9972));
#3348=EDGE_LOOP('',(#9973,#9974,#9975,#9976));
#3349=EDGE_LOOP('',(#9977,#9978,#9979,#9980));
#3350=EDGE_LOOP('',(#9981,#9982,#9983,#9984));
#3351=EDGE_LOOP('',(#9985));
#3352=EDGE_LOOP('',(#9986));
#3353=EDGE_LOOP('',(#9987));
#3354=EDGE_LOOP('',(#9988));
#3355=EDGE_LOOP('',(#9989));
#3356=EDGE_LOOP('',(#9990));
#3357=EDGE_LOOP('',(#9991));
#3358=EDGE_LOOP('',(#9992));
#3359=EDGE_LOOP('',(#9993));
#3360=EDGE_LOOP('',(#9994));
#3361=EDGE_LOOP('',(#9995));
#3362=EDGE_LOOP('',(#9996));
#3363=EDGE_LOOP('',(#9997));
#3364=EDGE_LOOP('',(#9998));
#3365=EDGE_LOOP('',(#9999,#10000,#10001,#10002));
#3366=EDGE_LOOP('',(#10003));
#3367=EDGE_LOOP('',(#10004,#10005,#10006,#10007));
#3368=EDGE_LOOP('',(#10008));
#3369=EDGE_LOOP('',(#10009));
#3370=EDGE_LOOP('',(#10010));
#3371=EDGE_LOOP('',(#10011,#10012,#10013,#10014));
#3372=EDGE_LOOP('',(#10015));
#3373=EDGE_LOOP('',(#10016,#10017,#10018,#10019));
#3374=EDGE_LOOP('',(#10020));
#3375=EDGE_LOOP('',(#10021));
#3376=EDGE_LOOP('',(#10022));
#3377=EDGE_LOOP('',(#10023,#10024,#10025,#10026));
#3378=EDGE_LOOP('',(#10027));
#3379=EDGE_LOOP('',(#10028,#10029,#10030,#10031));
#3380=EDGE_LOOP('',(#10032));
#3381=EDGE_LOOP('',(#10033));
#3382=EDGE_LOOP('',(#10034));
#3383=EDGE_LOOP('',(#10035,#10036,#10037,#10038));
#3384=EDGE_LOOP('',(#10039));
#3385=EDGE_LOOP('',(#10040,#10041,#10042,#10043));
#3386=EDGE_LOOP('',(#10044));
#3387=EDGE_LOOP('',(#10045,#10046,#10047,#10048));
#3388=EDGE_LOOP('',(#10049,#10050,#10051,#10052));
#3389=EDGE_LOOP('',(#10053,#10054,#10055,#10056));
#3390=EDGE_LOOP('',(#10057,#10058,#10059,#10060));
#3391=EDGE_LOOP('',(#10061,#10062,#10063,#10064));
#3392=EDGE_LOOP('',(#10065,#10066,#10067,#10068));
#3393=EDGE_LOOP('',(#10069));
#3394=EDGE_LOOP('',(#10070));
#3395=EDGE_LOOP('',(#10071));
#3396=EDGE_LOOP('',(#10072));
#3397=EDGE_LOOP('',(#10073));
#3398=EDGE_LOOP('',(#10074));
#3399=EDGE_LOOP('',(#10075));
#3400=EDGE_LOOP('',(#10076));
#3401=EDGE_LOOP('',(#10077));
#3402=EDGE_LOOP('',(#10078));
#3403=EDGE_LOOP('',(#10079));
#3404=EDGE_LOOP('',(#10080));
#3405=EDGE_LOOP('',(#10081));
#3406=EDGE_LOOP('',(#10082));
#3407=EDGE_LOOP('',(#10083,#10084,#10085,#10086));
#3408=EDGE_LOOP('',(#10087));
#3409=EDGE_LOOP('',(#10088,#10089,#10090,#10091));
#3410=EDGE_LOOP('',(#10092));
#3411=EDGE_LOOP('',(#10093));
#3412=EDGE_LOOP('',(#10094));
#3413=EDGE_LOOP('',(#10095,#10096,#10097,#10098));
#3414=EDGE_LOOP('',(#10099));
#3415=EDGE_LOOP('',(#10100,#10101,#10102,#10103));
#3416=EDGE_LOOP('',(#10104));
#3417=EDGE_LOOP('',(#10105));
#3418=EDGE_LOOP('',(#10106));
#3419=EDGE_LOOP('',(#10107,#10108,#10109,#10110));
#3420=EDGE_LOOP('',(#10111));
#3421=EDGE_LOOP('',(#10112,#10113,#10114,#10115));
#3422=EDGE_LOOP('',(#10116));
#3423=EDGE_LOOP('',(#10117));
#3424=EDGE_LOOP('',(#10118));
#3425=EDGE_LOOP('',(#10119,#10120,#10121,#10122));
#3426=EDGE_LOOP('',(#10123));
#3427=EDGE_LOOP('',(#10124,#10125,#10126,#10127));
#3428=EDGE_LOOP('',(#10128));
#3429=EDGE_LOOP('',(#10129,#10130,#10131,#10132));
#3430=EDGE_LOOP('',(#10133,#10134,#10135,#10136));
#3431=EDGE_LOOP('',(#10137,#10138,#10139,#10140));
#3432=EDGE_LOOP('',(#10141,#10142,#10143,#10144));
#3433=EDGE_LOOP('',(#10145,#10146,#10147,#10148));
#3434=EDGE_LOOP('',(#10149,#10150,#10151,#10152));
#3435=EDGE_LOOP('',(#10153));
#3436=EDGE_LOOP('',(#10154));
#3437=EDGE_LOOP('',(#10155));
#3438=EDGE_LOOP('',(#10156));
#3439=EDGE_LOOP('',(#10157));
#3440=EDGE_LOOP('',(#10158));
#3441=EDGE_LOOP('',(#10159));
#3442=EDGE_LOOP('',(#10160));
#3443=EDGE_LOOP('',(#10161));
#3444=EDGE_LOOP('',(#10162));
#3445=EDGE_LOOP('',(#10163));
#3446=EDGE_LOOP('',(#10164));
#3447=EDGE_LOOP('',(#10165));
#3448=EDGE_LOOP('',(#10166));
#3449=EDGE_LOOP('',(#10167,#10168,#10169,#10170));
#3450=EDGE_LOOP('',(#10171));
#3451=EDGE_LOOP('',(#10172,#10173,#10174,#10175));
#3452=EDGE_LOOP('',(#10176));
#3453=EDGE_LOOP('',(#10177));
#3454=EDGE_LOOP('',(#10178));
#3455=EDGE_LOOP('',(#10179,#10180,#10181,#10182));
#3456=EDGE_LOOP('',(#10183));
#3457=EDGE_LOOP('',(#10184,#10185,#10186,#10187));
#3458=EDGE_LOOP('',(#10188));
#3459=EDGE_LOOP('',(#10189));
#3460=EDGE_LOOP('',(#10190));
#3461=EDGE_LOOP('',(#10191,#10192,#10193,#10194));
#3462=EDGE_LOOP('',(#10195));
#3463=EDGE_LOOP('',(#10196,#10197,#10198,#10199));
#3464=EDGE_LOOP('',(#10200));
#3465=EDGE_LOOP('',(#10201));
#3466=EDGE_LOOP('',(#10202));
#3467=EDGE_LOOP('',(#10203,#10204,#10205,#10206));
#3468=EDGE_LOOP('',(#10207));
#3469=EDGE_LOOP('',(#10208,#10209,#10210,#10211));
#3470=EDGE_LOOP('',(#10212));
#3471=EDGE_LOOP('',(#10213,#10214,#10215,#10216,#10217,#10218));
#3472=EDGE_LOOP('',(#10219,#10220,#10221,#10222,#10223));
#3473=EDGE_LOOP('',(#10224,#10225,#10226,#10227));
#3474=EDGE_LOOP('',(#10228,#10229,#10230,#10231));
#3475=EDGE_LOOP('',(#10232));
#3476=EDGE_LOOP('',(#10233));
#3477=EDGE_LOOP('',(#10234,#10235,#10236,#10237,#10238));
#3478=EDGE_LOOP('',(#10239));
#3479=EDGE_LOOP('',(#10240));
#3480=EDGE_LOOP('',(#10241,#10242,#10243,#10244));
#3481=EDGE_LOOP('',(#10245,#10246,#10247,#10248,#10249,#10250));
#3482=EDGE_LOOP('',(#10251,#10252,#10253,#10254,#10255));
#3483=EDGE_LOOP('',(#10256));
#3484=EDGE_LOOP('',(#10257));
#3485=EDGE_LOOP('',(#10258,#10259,#10260,#10261));
#3486=EDGE_LOOP('',(#10262,#10263,#10264,#10265));
#3487=EDGE_LOOP('',(#10266,#10267,#10268,#10269));
#3488=EDGE_LOOP('',(#10270));
#3489=EDGE_LOOP('',(#10271));
#3490=EDGE_LOOP('',(#10272,#10273,#10274,#10275,#10276));
#3491=EDGE_LOOP('',(#10277,#10278));
#3492=EDGE_LOOP('',(#10279,#10280));
#3493=EDGE_LOOP('',(#10281,#10282));
#3494=EDGE_LOOP('',(#10283,#10284));
#3495=EDGE_LOOP('',(#10285,#10286));
#3496=EDGE_LOOP('',(#10287,#10288));
#3497=EDGE_LOOP('',(#10289,#10290));
#3498=EDGE_LOOP('',(#10291,#10292,#10293,#10294));
#3499=EDGE_LOOP('',(#10295,#10296,#10297,#10298,#10299,#10300,#10301,#10302,
#10303,#10304,#10305,#10306,#10307,#10308,#10309,#10310,#10311,#10312));
#3500=EDGE_LOOP('',(#10313,#10314,#10315,#10316));
#3501=EDGE_LOOP('',(#10317,#10318,#10319,#10320));
#3502=EDGE_LOOP('',(#10321,#10322,#10323,#10324));
#3503=EDGE_LOOP('',(#10325,#10326,#10327,#10328));
#3504=EDGE_LOOP('',(#10329,#10330,#10331,#10332,#10333,#10334));
#3505=EDGE_LOOP('',(#10335,#10336,#10337,#10338));
#3506=EDGE_LOOP('',(#10339,#10340,#10341,#10342));
#3507=EDGE_LOOP('',(#10343,#10344,#10345,#10346));
#3508=EDGE_LOOP('',(#10347,#10348,#10349,#10350));
#3509=EDGE_LOOP('',(#10351,#10352,#10353,#10354));
#3510=EDGE_LOOP('',(#10355,#10356,#10357,#10358,#10359,#10360,#10361,#10362,
#10363,#10364,#10365,#10366,#10367,#10368,#10369,#10370,#10371,#10372));
#3511=EDGE_LOOP('',(#10373,#10374,#10375,#10376));
#3512=EDGE_LOOP('',(#10377,#10378,#10379,#10380));
#3513=EDGE_LOOP('',(#10381));
#3514=EDGE_LOOP('',(#10382));
#3515=EDGE_LOOP('',(#10383,#10384,#10385,#10386));
#3516=EDGE_LOOP('',(#10387));
#3517=EDGE_LOOP('',(#10388));
#3518=EDGE_LOOP('',(#10389,#10390,#10391,#10392));
#3519=EDGE_LOOP('',(#10393));
#3520=EDGE_LOOP('',(#10394));
#3521=EDGE_LOOP('',(#10395,#10396,#10397,#10398));
#3522=EDGE_LOOP('',(#10399));
#3523=EDGE_LOOP('',(#10400));
#3524=EDGE_LOOP('',(#10401,#10402,#10403,#10404));
#3525=EDGE_LOOP('',(#10405));
#3526=EDGE_LOOP('',(#10406));
#3527=EDGE_LOOP('',(#10407,#10408,#10409,#10410));
#3528=EDGE_LOOP('',(#10411,#10412,#10413,#10414));
#3529=EDGE_LOOP('',(#10415,#10416,#10417,#10418));
#3530=EDGE_LOOP('',(#10419,#10420,#10421,#10422));
#3531=EDGE_LOOP('',(#10423,#10424,#10425,#10426));
#3532=EDGE_LOOP('',(#10427,#10428,#10429,#10430));
#3533=EDGE_LOOP('',(#10431,#10432,#10433,#10434));
#3534=EDGE_LOOP('',(#10435,#10436,#10437,#10438));
#3535=EDGE_LOOP('',(#10439,#10440,#10441,#10442));
#3536=EDGE_LOOP('',(#10443,#10444,#10445,#10446));
#3537=EDGE_LOOP('',(#10447,#10448,#10449,#10450));
#3538=EDGE_LOOP('',(#10451,#10452,#10453,#10454));
#3539=EDGE_LOOP('',(#10455,#10456,#10457,#10458));
#3540=EDGE_LOOP('',(#10459,#10460,#10461,#10462));
#3541=EDGE_LOOP('',(#10463,#10464,#10465,#10466,#10467,#10468,#10469,#10470,
#10471,#10472,#10473));
#3542=EDGE_LOOP('',(#10474));
#3543=EDGE_LOOP('',(#10475));
#3544=EDGE_LOOP('',(#10476));
#3545=EDGE_LOOP('',(#10477));
#3546=EDGE_LOOP('',(#10478));
#3547=EDGE_LOOP('',(#10479));
#3548=EDGE_LOOP('',(#10480));
#3549=EDGE_LOOP('',(#10481));
#3550=EDGE_LOOP('',(#10482,#10483,#10484,#10485));
#3551=EDGE_LOOP('',(#10486,#10487,#10488,#10489));
#3552=EDGE_LOOP('',(#10490,#10491,#10492,#10493));
#3553=EDGE_LOOP('',(#10494,#10495,#10496,#10497));
#3554=EDGE_LOOP('',(#10498,#10499,#10500,#10501));
#3555=EDGE_LOOP('',(#10502,#10503,#10504,#10505));
#3556=EDGE_LOOP('',(#10506,#10507,#10508,#10509,#10510,#10511,#10512,#10513,
#10514,#10515,#10516));
#3557=EDGE_LOOP('',(#10517));
#3558=EDGE_LOOP('',(#10518));
#3559=EDGE_LOOP('',(#10519));
#3560=EDGE_LOOP('',(#10520));
#3561=EDGE_LOOP('',(#10521));
#3562=EDGE_LOOP('',(#10522));
#3563=EDGE_LOOP('',(#10523));
#3564=EDGE_LOOP('',(#10524));
#3565=EDGE_LOOP('',(#10525,#10526,#10527,#10528));
#3566=EDGE_LOOP('',(#10529,#10530,#10531,#10532));
#3567=EDGE_LOOP('',(#10533,#10534,#10535,#10536));
#3568=EDGE_LOOP('',(#10537,#10538,#10539,#10540));
#3569=EDGE_LOOP('',(#10541,#10542,#10543,#10544));
#3570=EDGE_LOOP('',(#10545,#10546,#10547,#10548));
#3571=EDGE_LOOP('',(#10549,#10550,#10551,#10552));
#3572=EDGE_LOOP('',(#10553,#10554,#10555,#10556));
#3573=EDGE_LOOP('',(#10557,#10558,#10559,#10560));
#3574=EDGE_LOOP('',(#10561,#10562,#10563,#10564));
#3575=EDGE_LOOP('',(#10565,#10566,#10567,#10568));
#3576=EDGE_LOOP('',(#10569,#10570,#10571,#10572));
#3577=EDGE_LOOP('',(#10573,#10574,#10575,#10576));
#3578=EDGE_LOOP('',(#10577,#10578,#10579,#10580));
#3579=EDGE_LOOP('',(#10581,#10582,#10583,#10584));
#3580=EDGE_LOOP('',(#10585,#10586,#10587,#10588));
#3581=EDGE_LOOP('',(#10589,#10590,#10591,#10592));
#3582=EDGE_LOOP('',(#10593,#10594,#10595,#10596));
#3583=EDGE_LOOP('',(#10597,#10598,#10599,#10600));
#3584=EDGE_LOOP('',(#10601));
#3585=EDGE_LOOP('',(#10602,#10603,#10604,#10605));
#3586=EDGE_LOOP('',(#10606,#10607,#10608,#10609));
#3587=EDGE_LOOP('',(#10610,#10611,#10612,#10613));
#3588=EDGE_LOOP('',(#10614));
#3589=EDGE_LOOP('',(#10615));
#3590=EDGE_LOOP('',(#10616));
#3591=EDGE_LOOP('',(#10617));
#3592=EDGE_LOOP('',(#10618));
#3593=EDGE_LOOP('',(#10619));
#3594=EDGE_LOOP('',(#10620));
#3595=EDGE_LOOP('',(#10621));
#3596=EDGE_LOOP('',(#10622));
#3597=EDGE_LOOP('',(#10623));
#3598=EDGE_LOOP('',(#10624,#10625,#10626,#10627));
#3599=EDGE_LOOP('',(#10628,#10629,#10630,#10631));
#3600=EDGE_LOOP('',(#10632,#10633,#10634,#10635));
#3601=EDGE_LOOP('',(#10636));
#3602=EDGE_LOOP('',(#10637));
#3603=EDGE_LOOP('',(#10638));
#3604=EDGE_LOOP('',(#10639,#10640,#10641,#10642));
#3605=EDGE_LOOP('',(#10643,#10644,#10645,#10646));
#3606=EDGE_LOOP('',(#10647));
#3607=EDGE_LOOP('',(#10648));
#3608=EDGE_LOOP('',(#10649));
#3609=EDGE_LOOP('',(#10650));
#3610=EDGE_LOOP('',(#10651,#10652,#10653,#10654));
#3611=EDGE_LOOP('',(#10655,#10656,#10657,#10658));
#3612=EDGE_LOOP('',(#10659));
#3613=EDGE_LOOP('',(#10660));
#3614=EDGE_LOOP('',(#10661));
#3615=EDGE_LOOP('',(#10662));
#3616=EDGE_LOOP('',(#10663,#10664,#10665,#10666));
#3617=EDGE_LOOP('',(#10667,#10668,#10669,#10670));
#3618=EDGE_LOOP('',(#10671));
#3619=EDGE_LOOP('',(#10672));
#3620=EDGE_LOOP('',(#10673));
#3621=EDGE_LOOP('',(#10674));
#3622=EDGE_LOOP('',(#10675,#10676,#10677,#10678));
#3623=EDGE_LOOP('',(#10679,#10680,#10681,#10682));
#3624=EDGE_LOOP('',(#10683));
#3625=EDGE_LOOP('',(#10684));
#3626=EDGE_LOOP('',(#10685));
#3627=EDGE_LOOP('',(#10686));
#3628=EDGE_LOOP('',(#10687,#10688,#10689,#10690));
#3629=EDGE_LOOP('',(#10691));
#3630=EDGE_LOOP('',(#10692,#10693,#10694,#10695));
#3631=EDGE_LOOP('',(#10696,#10697,#10698,#10699));
#3632=EDGE_LOOP('',(#10700,#10701,#10702,#10703));
#3633=EDGE_LOOP('',(#10704));
#3634=EDGE_LOOP('',(#10705));
#3635=EDGE_LOOP('',(#10706));
#3636=EDGE_LOOP('',(#10707));
#3637=EDGE_LOOP('',(#10708));
#3638=EDGE_LOOP('',(#10709));
#3639=EDGE_LOOP('',(#10710));
#3640=EDGE_LOOP('',(#10711));
#3641=EDGE_LOOP('',(#10712));
#3642=EDGE_LOOP('',(#10713));
#3643=EDGE_LOOP('',(#10714,#10715,#10716,#10717));
#3644=EDGE_LOOP('',(#10718,#10719,#10720,#10721));
#3645=EDGE_LOOP('',(#10722,#10723,#10724,#10725));
#3646=EDGE_LOOP('',(#10726));
#3647=EDGE_LOOP('',(#10727));
#3648=EDGE_LOOP('',(#10728));
#3649=EDGE_LOOP('',(#10729,#10730,#10731,#10732));
#3650=EDGE_LOOP('',(#10733,#10734,#10735,#10736));
#3651=EDGE_LOOP('',(#10737));
#3652=EDGE_LOOP('',(#10738));
#3653=EDGE_LOOP('',(#10739));
#3654=EDGE_LOOP('',(#10740));
#3655=EDGE_LOOP('',(#10741,#10742,#10743,#10744));
#3656=EDGE_LOOP('',(#10745,#10746,#10747,#10748));
#3657=EDGE_LOOP('',(#10749));
#3658=EDGE_LOOP('',(#10750));
#3659=EDGE_LOOP('',(#10751));
#3660=EDGE_LOOP('',(#10752));
#3661=EDGE_LOOP('',(#10753,#10754,#10755,#10756));
#3662=EDGE_LOOP('',(#10757,#10758,#10759,#10760));
#3663=EDGE_LOOP('',(#10761));
#3664=EDGE_LOOP('',(#10762));
#3665=EDGE_LOOP('',(#10763));
#3666=EDGE_LOOP('',(#10764));
#3667=EDGE_LOOP('',(#10765));
#3668=EDGE_LOOP('',(#10766,#10767,#10768,#10769));
#3669=EDGE_LOOP('',(#10770,#10771,#10772,#10773));
#3670=EDGE_LOOP('',(#10774,#10775,#10776,#10777));
#3671=EDGE_LOOP('',(#10778));
#3672=EDGE_LOOP('',(#10779));
#3673=EDGE_LOOP('',(#10780,#10781,#10782,#10783));
#3674=EDGE_LOOP('',(#10784,#10785,#10786,#10787));
#3675=EDGE_LOOP('',(#10788,#10789,#10790,#10791));
#3676=EDGE_LOOP('',(#10792));
#3677=EDGE_LOOP('',(#10793,#10794,#10795,#10796));
#3678=EDGE_LOOP('',(#10797,#10798,#10799,#10800));
#3679=EDGE_LOOP('',(#10801,#10802,#10803,#10804));
#3680=EDGE_LOOP('',(#10805,#10806,#10807,#10808));
#3681=EDGE_LOOP('',(#10809,#10810,#10811,#10812));
#3682=EDGE_LOOP('',(#10813,#10814,#10815,#10816));
#3683=EDGE_LOOP('',(#10817,#10818,#10819,#10820,#10821,#10822));
#3684=EDGE_LOOP('',(#10823,#10824,#10825,#10826,#10827,#10828));
#3685=EDGE_LOOP('',(#10829,#10830,#10831,#10832));
#3686=EDGE_LOOP('',(#10833,#10834,#10835,#10836));
#3687=EDGE_LOOP('',(#10837,#10838,#10839,#10840));
#3688=EDGE_LOOP('',(#10841,#10842,#10843,#10844));
#3689=EDGE_LOOP('',(#10845,#10846,#10847,#10848));
#3690=EDGE_LOOP('',(#10849));
#3691=EDGE_LOOP('',(#10850));
#3692=EDGE_LOOP('',(#10851));
#3693=EDGE_LOOP('',(#10852,#10853,#10854,#10855));
#3694=EDGE_LOOP('',(#10856,#10857,#10858,#10859));
#3695=EDGE_LOOP('',(#10860));
#3696=EDGE_LOOP('',(#10861));
#3697=EDGE_LOOP('',(#10862));
#3698=EDGE_LOOP('',(#10863,#10864,#10865,#10866));
#3699=EDGE_LOOP('',(#10867,#10868,#10869,#10870));
#3700=EDGE_LOOP('',(#10871,#10872,#10873,#10874));
#3701=EDGE_LOOP('',(#10875,#10876,#10877,#10878));
#3702=EDGE_LOOP('',(#10879,#10880,#10881,#10882));
#3703=EDGE_LOOP('',(#10883,#10884,#10885,#10886));
#3704=EDGE_LOOP('',(#10887,#10888,#10889,#10890));
#3705=EDGE_LOOP('',(#10891,#10892,#10893,#10894));
#3706=EDGE_LOOP('',(#10895,#10896,#10897,#10898));
#3707=EDGE_LOOP('',(#10899,#10900,#10901,#10902));
#3708=EDGE_LOOP('',(#10903));
#3709=EDGE_LOOP('',(#10904));
#3710=EDGE_LOOP('',(#10905));
#3711=EDGE_LOOP('',(#10906,#10907,#10908,#10909));
#3712=EDGE_LOOP('',(#10910));
#3713=EDGE_LOOP('',(#10911));
#3714=EDGE_LOOP('',(#10912));
#3715=EDGE_LOOP('',(#10913,#10914,#10915,#10916));
#3716=EDGE_LOOP('',(#10917,#10918,#10919,#10920));
#3717=EDGE_LOOP('',(#10921,#10922,#10923,#10924));
#3718=EDGE_LOOP('',(#10925,#10926,#10927,#10928));
#3719=EDGE_LOOP('',(#10929,#10930,#10931,#10932));
#3720=EDGE_LOOP('',(#10933,#10934,#10935,#10936));
#3721=EDGE_LOOP('',(#10937,#10938,#10939,#10940));
#3722=EDGE_LOOP('',(#10941,#10942,#10943,#10944));
#3723=EDGE_LOOP('',(#10945));
#3724=EDGE_LOOP('',(#10946));
#3725=EDGE_LOOP('',(#10947));
#3726=EDGE_LOOP('',(#10948,#10949,#10950,#10951));
#3727=EDGE_LOOP('',(#10952));
#3728=EDGE_LOOP('',(#10953));
#3729=EDGE_LOOP('',(#10954));
#3730=EDGE_LOOP('',(#10955,#10956,#10957,#10958));
#3731=EDGE_LOOP('',(#10959,#10960,#10961,#10962));
#3732=EDGE_LOOP('',(#10963));
#3733=EDGE_LOOP('',(#10964,#10965,#10966,#10967));
#3734=EDGE_LOOP('',(#10968,#10969,#10970,#10971));
#3735=EDGE_LOOP('',(#10972));
#3736=EDGE_LOOP('',(#10973,#10974,#10975,#10976));
#3737=EDGE_LOOP('',(#10977,#10978,#10979,#10980));
#3738=EDGE_LOOP('',(#10981,#10982,#10983,#10984));
#3739=EDGE_LOOP('',(#10985,#10986,#10987,#10988));
#3740=EDGE_LOOP('',(#10989));
#3741=EDGE_LOOP('',(#10990));
#3742=EDGE_LOOP('',(#10991));
#3743=EDGE_LOOP('',(#10992,#10993,#10994,#10995));
#3744=EDGE_LOOP('',(#10996));
#3745=EDGE_LOOP('',(#10997,#10998,#10999,#11000));
#3746=EDGE_LOOP('',(#11001));
#3747=EDGE_LOOP('',(#11002));
#3748=EDGE_LOOP('',(#11003,#11004,#11005,#11006));
#3749=EDGE_LOOP('',(#11007,#11008,#11009,#11010));
#3750=EDGE_LOOP('',(#11011));
#3751=EDGE_LOOP('',(#11012));
#3752=EDGE_LOOP('',(#11013));
#3753=EDGE_LOOP('',(#11014));
#3754=EDGE_LOOP('',(#11015,#11016,#11017,#11018));
#3755=EDGE_LOOP('',(#11019,#11020,#11021,#11022));
#3756=EDGE_LOOP('',(#11023));
#3757=EDGE_LOOP('',(#11024));
#3758=EDGE_LOOP('',(#11025));
#3759=EDGE_LOOP('',(#11026));
#3760=EDGE_LOOP('',(#11027,#11028,#11029,#11030));
#3761=EDGE_LOOP('',(#11031,#11032,#11033,#11034));
#3762=EDGE_LOOP('',(#11035,#11036,#11037,#11038));
#3763=EDGE_LOOP('',(#11039,#11040,#11041,#11042));
#3764=EDGE_LOOP('',(#11043,#11044,#11045,#11046));
#3765=EDGE_LOOP('',(#11047));
#3766=EDGE_LOOP('',(#11048));
#3767=EDGE_LOOP('',(#11049,#11050,#11051,#11052));
#3768=EDGE_LOOP('',(#11053));
#3769=EDGE_LOOP('',(#11054));
#3770=EDGE_LOOP('',(#11055,#11056,#11057,#11058));
#3771=EDGE_LOOP('',(#11059));
#3772=EDGE_LOOP('',(#11060));
#3773=EDGE_LOOP('',(#11061,#11062,#11063,#11064));
#3774=EDGE_LOOP('',(#11065));
#3775=EDGE_LOOP('',(#11066));
#3776=EDGE_LOOP('',(#11067,#11068,#11069,#11070));
#3777=EDGE_LOOP('',(#11071));
#3778=EDGE_LOOP('',(#11072));
#3779=EDGE_LOOP('',(#11073,#11074,#11075,#11076));
#3780=EDGE_LOOP('',(#11077));
#3781=EDGE_LOOP('',(#11078));
#3782=EDGE_LOOP('',(#11079,#11080,#11081,#11082));
#3783=EDGE_LOOP('',(#11083,#11084,#11085,#11086));
#3784=EDGE_LOOP('',(#11087,#11088,#11089,#11090));
#3785=EDGE_LOOP('',(#11091,#11092,#11093,#11094));
#3786=EDGE_LOOP('',(#11095,#11096,#11097,#11098));
#3787=EDGE_LOOP('',(#11099,#11100,#11101,#11102));
#3788=EDGE_LOOP('',(#11103));
#3789=EDGE_LOOP('',(#11104));
#3790=EDGE_LOOP('',(#11105,#11106,#11107,#11108));
#3791=EDGE_LOOP('',(#11109,#11110,#11111,#11112));
#3792=EDGE_LOOP('',(#11113));
#3793=EDGE_LOOP('',(#11114));
#3794=EDGE_LOOP('',(#11115,#11116,#11117,#11118));
#3795=EDGE_LOOP('',(#11119,#11120,#11121,#11122));
#3796=EDGE_LOOP('',(#11123,#11124,#11125,#11126));
#3797=EDGE_LOOP('',(#11127,#11128,#11129,#11130));
#3798=EDGE_LOOP('',(#11131,#11132,#11133,#11134));
#3799=EDGE_LOOP('',(#11135,#11136,#11137,#11138));
#3800=EDGE_LOOP('',(#11139,#11140,#11141,#11142));
#3801=EDGE_LOOP('',(#11143,#11144,#11145,#11146));
#3802=EDGE_LOOP('',(#11147,#11148,#11149,#11150,#11151,#11152));
#3803=EDGE_LOOP('',(#11153,#11154,#11155,#11156,#11157,#11158));
#3804=EDGE_LOOP('',(#11159));
#3805=EDGE_LOOP('',(#11160));
#3806=EDGE_LOOP('',(#11161,#11162,#11163,#11164));
#3807=EDGE_LOOP('',(#11165,#11166,#11167,#11168));
#3808=EDGE_LOOP('',(#11169,#11170,#11171,#11172));
#3809=EDGE_LOOP('',(#11173));
#3810=EDGE_LOOP('',(#11174));
#3811=EDGE_LOOP('',(#11175,#11176,#11177,#11178));
#3812=EDGE_LOOP('',(#11179,#11180,#11181,#11182));
#3813=EDGE_LOOP('',(#11183,#11184,#11185,#11186));
#3814=EDGE_LOOP('',(#11187,#11188,#11189,#11190));
#3815=EDGE_LOOP('',(#11191,#11192,#11193,#11194));
#3816=EDGE_LOOP('',(#11195));
#3817=EDGE_LOOP('',(#11196));
#3818=EDGE_LOOP('',(#11197,#11198,#11199,#11200));
#3819=EDGE_LOOP('',(#11201,#11202,#11203,#11204));
#3820=EDGE_LOOP('',(#11205,#11206,#11207,#11208));
#3821=EDGE_LOOP('',(#11209,#11210,#11211,#11212));
#3822=EDGE_LOOP('',(#11213,#11214,#11215,#11216));
#3823=EDGE_LOOP('',(#11217));
#3824=EDGE_LOOP('',(#11218));
#3825=EDGE_LOOP('',(#11219,#11220,#11221,#11222));
#3826=EDGE_LOOP('',(#11223));
#3827=EDGE_LOOP('',(#11224));
#3828=EDGE_LOOP('',(#11225,#11226,#11227,#11228));
#3829=EDGE_LOOP('',(#11229,#11230,#11231,#11232));
#3830=EDGE_LOOP('',(#11233));
#3831=EDGE_LOOP('',(#11234));
#3832=EDGE_LOOP('',(#11235));
#3833=EDGE_LOOP('',(#11236));
#3834=EDGE_LOOP('',(#11237,#11238,#11239,#11240));
#3835=EDGE_LOOP('',(#11241,#11242,#11243,#11244));
#3836=EDGE_LOOP('',(#11245));
#3837=EDGE_LOOP('',(#11246));
#3838=EDGE_LOOP('',(#11247));
#3839=EDGE_LOOP('',(#11248));
#3840=EDGE_LOOP('',(#11249,#11250,#11251,#11252));
#3841=EDGE_LOOP('',(#11253,#11254,#11255,#11256));
#3842=EDGE_LOOP('',(#11257));
#3843=EDGE_LOOP('',(#11258));
#3844=EDGE_LOOP('',(#11259));
#3845=EDGE_LOOP('',(#11260));
#3846=EDGE_LOOP('',(#11261,#11262,#11263,#11264));
#3847=EDGE_LOOP('',(#11265));
#3848=EDGE_LOOP('',(#11266));
#3849=LINE('',#19752,#4524);
#3850=LINE('',#19758,#4525);
#3851=LINE('',#19764,#4526);
#3852=LINE('',#19770,#4527);
#3853=LINE('',#19776,#4528);
#3854=LINE('',#19782,#4529);
#3855=LINE('',#19788,#4530);
#3856=LINE('',#19794,#4531);
#3857=LINE('',#19800,#4532);
#3858=LINE('',#19806,#4533);
#3859=LINE('',#19812,#4534);
#3860=LINE('',#19818,#4535);
#3861=LINE('',#19823,#4536);
#3862=LINE('',#19825,#4537);
#3863=LINE('',#19827,#4538);
#3864=LINE('',#19828,#4539);
#3865=LINE('',#19831,#4540);
#3866=LINE('',#19833,#4541);
#3867=LINE('',#19834,#4542);
#3868=LINE('',#19837,#4543);
#3869=LINE('',#19839,#4544);
#3870=LINE('',#19840,#4545);
#3871=LINE('',#19842,#4546);
#3872=LINE('',#19843,#4547);
#3873=LINE('',#19850,#4548);
#3874=LINE('',#19852,#4549);
#3875=LINE('',#19854,#4550);
#3876=LINE('',#19855,#4551);
#3877=LINE('',#19858,#4552);
#3878=LINE('',#19860,#4553);
#3879=LINE('',#19861,#4554);
#3880=LINE('',#19864,#4555);
#3881=LINE('',#19866,#4556);
#3882=LINE('',#19867,#4557);
#3883=LINE('',#19869,#4558);
#3884=LINE('',#19870,#4559);
#3885=LINE('',#19877,#4560);
#3886=LINE('',#19879,#4561);
#3887=LINE('',#19881,#4562);
#3888=LINE('',#19882,#4563);
#3889=LINE('',#19885,#4564);
#3890=LINE('',#19887,#4565);
#3891=LINE('',#19888,#4566);
#3892=LINE('',#19891,#4567);
#3893=LINE('',#19893,#4568);
#3894=LINE('',#19894,#4569);
#3895=LINE('',#19896,#4570);
#3896=LINE('',#19897,#4571);
#3897=LINE('',#19905,#4572);
#3898=LINE('',#19911,#4573);
#3899=LINE('',#19917,#4574);
#3900=LINE('',#19923,#4575);
#3901=LINE('',#19929,#4576);
#3902=LINE('',#19935,#4577);
#3903=LINE('',#19941,#4578);
#3904=LINE('',#19947,#4579);
#3905=LINE('',#19952,#4580);
#3906=LINE('',#19954,#4581);
#3907=LINE('',#19956,#4582);
#3908=LINE('',#19958,#4583);
#3909=LINE('',#19960,#4584);
#3910=LINE('',#19962,#4585);
#3911=LINE('',#19964,#4586);
#3912=LINE('',#19965,#4587);
#3913=LINE('',#19968,#4588);
#3914=LINE('',#19970,#4589);
#3915=LINE('',#19971,#4590);
#3916=LINE('',#19974,#4591);
#3917=LINE('',#19976,#4592);
#3918=LINE('',#19977,#4593);
#3919=LINE('',#19979,#4594);
#3920=LINE('',#19982,#4595);
#3921=LINE('',#19984,#4596);
#3922=LINE('',#19985,#4597);
#3923=LINE('',#19986,#4598);
#3924=LINE('',#19989,#4599);
#3925=LINE('',#19990,#4600);
#3926=LINE('',#19993,#4601);
#3927=LINE('',#19994,#4602);
#3928=LINE('',#19996,#4603);
#3929=LINE('',#20004,#4604);
#3930=LINE('',#20010,#4605);
#3931=LINE('',#20016,#4606);
#3932=LINE('',#20022,#4607);
#3933=LINE('',#20028,#4608);
#3934=LINE('',#20034,#4609);
#3935=LINE('',#20040,#4610);
#3936=LINE('',#20046,#4611);
#3937=LINE('',#20051,#4612);
#3938=LINE('',#20053,#4613);
#3939=LINE('',#20055,#4614);
#3940=LINE('',#20057,#4615);
#3941=LINE('',#20059,#4616);
#3942=LINE('',#20061,#4617);
#3943=LINE('',#20063,#4618);
#3944=LINE('',#20064,#4619);
#3945=LINE('',#20067,#4620);
#3946=LINE('',#20069,#4621);
#3947=LINE('',#20070,#4622);
#3948=LINE('',#20073,#4623);
#3949=LINE('',#20075,#4624);
#3950=LINE('',#20076,#4625);
#3951=LINE('',#20078,#4626);
#3952=LINE('',#20081,#4627);
#3953=LINE('',#20083,#4628);
#3954=LINE('',#20084,#4629);
#3955=LINE('',#20085,#4630);
#3956=LINE('',#20088,#4631);
#3957=LINE('',#20089,#4632);
#3958=LINE('',#20092,#4633);
#3959=LINE('',#20093,#4634);
#3960=LINE('',#20095,#4635);
#3961=LINE('',#20103,#4636);
#3962=LINE('',#20110,#4637);
#3963=LINE('',#20116,#4638);
#3964=LINE('',#20122,#4639);
#3965=LINE('',#20135,#4640);
#3966=LINE('',#20138,#4641);
#3967=LINE('',#20143,#4642);
#3968=LINE('',#20151,#4643);
#3969=LINE('',#20157,#4644);
#3970=LINE('',#20166,#4645);
#3971=LINE('',#20172,#4646);
#3972=LINE('',#20181,#4647);
#3973=LINE('',#20187,#4648);
#3974=LINE('',#20196,#4649);
#3975=LINE('',#20203,#4650);
#3976=LINE('',#20209,#4651);
#3977=LINE('',#20215,#4652);
#3978=LINE('',#20228,#4653);
#3979=LINE('',#20231,#4654);
#3980=LINE('',#20236,#4655);
#3981=LINE('',#20244,#4656);
#3982=LINE('',#20250,#4657);
#3983=LINE('',#20259,#4658);
#3984=LINE('',#20265,#4659);
#3985=LINE('',#20274,#4660);
#3986=LINE('',#20280,#4661);
#3987=LINE('',#20290,#4662);
#3988=LINE('',#20293,#4663);
#3989=LINE('',#20298,#4664);
#3990=LINE('',#20302,#4665);
#3991=LINE('',#20304,#4666);
#3992=LINE('',#20305,#4667);
#3993=LINE('',#20310,#4668);
#3994=LINE('',#20312,#4669);
#3995=LINE('',#20314,#4670);
#3996=LINE('',#20315,#4671);
#3997=LINE('',#20326,#4672);
#3998=LINE('',#20334,#4673);
#3999=LINE('',#20338,#4674);
#4000=LINE('',#20345,#4675);
#4001=LINE('',#20349,#4676);
#4002=LINE('',#20353,#4677);
#4003=LINE('',#20357,#4678);
#4004=LINE('',#20360,#4679);
#4005=LINE('',#20362,#4680);
#4006=LINE('',#20363,#4681);
#4007=LINE('',#20366,#4682);
#4008=LINE('',#20367,#4683);
#4009=LINE('',#20369,#4684);
#4010=LINE('',#20370,#4685);
#4011=LINE('',#20378,#4686);
#4012=LINE('',#20384,#4687);
#4013=LINE('',#20389,#4688);
#4014=LINE('',#20393,#4689);
#4015=LINE('',#20398,#4690);
#4016=LINE('',#20402,#4691);
#4017=LINE('',#20415,#4692);
#4018=LINE('',#20426,#4693);
#4019=LINE('',#20432,#4694);
#4020=LINE('',#20442,#4695);
#4021=LINE('',#20448,#4696);
#4022=LINE('',#20455,#4697);
#4023=LINE('',#20461,#4698);
#4024=LINE('',#20466,#4699);
#4025=LINE('',#20470,#4700);
#4026=LINE('',#20475,#4701);
#4027=LINE('',#20479,#4702);
#4028=LINE('',#20492,#4703);
#4029=LINE('',#20504,#4704);
#4030=LINE('',#20508,#4705);
#4031=LINE('',#20520,#4706);
#4032=LINE('',#20524,#4707);
#4033=LINE('',#20533,#4708);
#4034=LINE('',#20536,#4709);
#4035=LINE('',#20541,#4710);
#4036=LINE('',#20545,#4711);
#4037=LINE('',#20547,#4712);
#4038=LINE('',#20548,#4713);
#4039=LINE('',#20553,#4714);
#4040=LINE('',#20555,#4715);
#4041=LINE('',#20557,#4716);
#4042=LINE('',#20558,#4717);
#4043=LINE('',#20569,#4718);
#4044=LINE('',#20577,#4719);
#4045=LINE('',#20581,#4720);
#4046=LINE('',#20588,#4721);
#4047=LINE('',#20592,#4722);
#4048=LINE('',#20596,#4723);
#4049=LINE('',#20600,#4724);
#4050=LINE('',#20603,#4725);
#4051=LINE('',#20605,#4726);
#4052=LINE('',#20606,#4727);
#4053=LINE('',#20609,#4728);
#4054=LINE('',#20610,#4729);
#4055=LINE('',#20612,#4730);
#4056=LINE('',#20613,#4731);
#4057=LINE('',#20621,#4732);
#4058=LINE('',#20627,#4733);
#4059=LINE('',#20632,#4734);
#4060=LINE('',#20636,#4735);
#4061=LINE('',#20641,#4736);
#4062=LINE('',#20645,#4737);
#4063=LINE('',#20658,#4738);
#4064=LINE('',#20669,#4739);
#4065=LINE('',#20675,#4740);
#4066=LINE('',#20685,#4741);
#4067=LINE('',#20691,#4742);
#4068=LINE('',#20698,#4743);
#4069=LINE('',#20704,#4744);
#4070=LINE('',#20709,#4745);
#4071=LINE('',#20713,#4746);
#4072=LINE('',#20718,#4747);
#4073=LINE('',#20722,#4748);
#4074=LINE('',#20735,#4749);
#4075=LINE('',#20747,#4750);
#4076=LINE('',#20751,#4751);
#4077=LINE('',#20763,#4752);
#4078=LINE('',#20767,#4753);
#4079=LINE('',#20775,#4754);
#4080=LINE('',#20784,#4755);
#4081=LINE('',#20795,#4756);
#4082=LINE('',#20799,#4757);
#4083=LINE('',#20803,#4758);
#4084=LINE('',#20810,#4759);
#4085=LINE('',#20814,#4760);
#4086=LINE('',#20818,#4761);
#4087=LINE('',#20823,#4762);
#4088=LINE('',#20825,#4763);
#4089=LINE('',#20827,#4764);
#4090=LINE('',#20828,#4765);
#4091=LINE('',#20831,#4766);
#4092=LINE('',#20833,#4767);
#4093=LINE('',#20834,#4768);
#4094=LINE('',#20837,#4769);
#4095=LINE('',#20839,#4770);
#4096=LINE('',#20840,#4771);
#4097=LINE('',#20843,#4772);
#4098=LINE('',#20845,#4773);
#4099=LINE('',#20846,#4774);
#4100=LINE('',#20849,#4775);
#4101=LINE('',#20851,#4776);
#4102=LINE('',#20852,#4777);
#4103=LINE('',#20854,#4778);
#4104=LINE('',#20855,#4779);
#4105=LINE('',#20864,#4780);
#4106=LINE('',#20870,#4781);
#4107=LINE('',#20876,#4782);
#4108=LINE('',#20882,#4783);
#4109=LINE('',#20888,#4784);
#4110=LINE('',#20893,#4785);
#4111=LINE('',#20897,#4786);
#4112=LINE('',#20901,#4787);
#4113=LINE('',#20904,#4788);
#4114=LINE('',#20917,#4789);
#4115=LINE('',#20918,#4790);
#4116=LINE('',#20921,#4791);
#4117=LINE('',#20925,#4792);
#4118=LINE('',#20929,#4793);
#4119=LINE('',#20933,#4794);
#4120=LINE('',#20937,#4795);
#4121=LINE('',#20941,#4796);
#4122=LINE('',#20944,#4797);
#4123=LINE('',#20951,#4798);
#4124=LINE('',#20957,#4799);
#4125=LINE('',#20963,#4800);
#4126=LINE('',#20969,#4801);
#4127=LINE('',#20975,#4802);
#4128=LINE('',#20981,#4803);
#4129=LINE('',#20993,#4804);
#4130=LINE('',#20999,#4805);
#4131=LINE('',#21009,#4806);
#4132=LINE('',#21015,#4807);
#4133=LINE('',#21025,#4808);
#4134=LINE('',#21031,#4809);
#4135=LINE('',#21041,#4810);
#4136=LINE('',#21047,#4811);
#4137=LINE('',#21054,#4812);
#4138=LINE('',#21060,#4813);
#4139=LINE('',#21066,#4814);
#4140=LINE('',#21072,#4815);
#4141=LINE('',#21078,#4816);
#4142=LINE('',#21084,#4817);
#4143=LINE('',#21097,#4818);
#4144=LINE('',#21101,#4819);
#4145=LINE('',#21113,#4820);
#4146=LINE('',#21117,#4821);
#4147=LINE('',#21129,#4822);
#4148=LINE('',#21133,#4823);
#4149=LINE('',#21145,#4824);
#4150=LINE('',#21149,#4825);
#4151=LINE('',#21157,#4826);
#4152=LINE('',#21163,#4827);
#4153=LINE('',#21169,#4828);
#4154=LINE('',#21175,#4829);
#4155=LINE('',#21181,#4830);
#4156=LINE('',#21187,#4831);
#4157=LINE('',#21199,#4832);
#4158=LINE('',#21205,#4833);
#4159=LINE('',#21215,#4834);
#4160=LINE('',#21221,#4835);
#4161=LINE('',#21231,#4836);
#4162=LINE('',#21237,#4837);
#4163=LINE('',#21247,#4838);
#4164=LINE('',#21253,#4839);
#4165=LINE('',#21260,#4840);
#4166=LINE('',#21266,#4841);
#4167=LINE('',#21272,#4842);
#4168=LINE('',#21278,#4843);
#4169=LINE('',#21284,#4844);
#4170=LINE('',#21290,#4845);
#4171=LINE('',#21303,#4846);
#4172=LINE('',#21307,#4847);
#4173=LINE('',#21319,#4848);
#4174=LINE('',#21323,#4849);
#4175=LINE('',#21335,#4850);
#4176=LINE('',#21339,#4851);
#4177=LINE('',#21351,#4852);
#4178=LINE('',#21355,#4853);
#4179=LINE('',#21364,#4854);
#4180=LINE('',#21370,#4855);
#4181=LINE('',#21376,#4856);
#4182=LINE('',#21382,#4857);
#4183=LINE('',#21388,#4858);
#4184=LINE('',#21393,#4859);
#4185=LINE('',#21397,#4860);
#4186=LINE('',#21401,#4861);
#4187=LINE('',#21403,#4862);
#4188=LINE('',#21404,#4863);
#4189=LINE('',#21407,#4864);
#4190=LINE('',#21422,#4865);
#4191=LINE('',#21426,#4866);
#4192=LINE('',#21430,#4867);
#4193=LINE('',#21434,#4868);
#4194=LINE('',#21438,#4869);
#4195=LINE('',#21441,#4870);
#4196=LINE('',#21444,#4871);
#4197=LINE('',#21451,#4872);
#4198=LINE('',#21457,#4873);
#4199=LINE('',#21463,#4874);
#4200=LINE('',#21469,#4875);
#4201=LINE('',#21475,#4876);
#4202=LINE('',#21481,#4877);
#4203=LINE('',#21493,#4878);
#4204=LINE('',#21499,#4879);
#4205=LINE('',#21509,#4880);
#4206=LINE('',#21515,#4881);
#4207=LINE('',#21525,#4882);
#4208=LINE('',#21531,#4883);
#4209=LINE('',#21541,#4884);
#4210=LINE('',#21547,#4885);
#4211=LINE('',#21554,#4886);
#4212=LINE('',#21560,#4887);
#4213=LINE('',#21566,#4888);
#4214=LINE('',#21572,#4889);
#4215=LINE('',#21578,#4890);
#4216=LINE('',#21584,#4891);
#4217=LINE('',#21597,#4892);
#4218=LINE('',#21601,#4893);
#4219=LINE('',#21613,#4894);
#4220=LINE('',#21617,#4895);
#4221=LINE('',#21629,#4896);
#4222=LINE('',#21633,#4897);
#4223=LINE('',#21645,#4898);
#4224=LINE('',#21649,#4899);
#4225=LINE('',#21657,#4900);
#4226=LINE('',#21663,#4901);
#4227=LINE('',#21669,#4902);
#4228=LINE('',#21675,#4903);
#4229=LINE('',#21681,#4904);
#4230=LINE('',#21687,#4905);
#4231=LINE('',#21699,#4906);
#4232=LINE('',#21705,#4907);
#4233=LINE('',#21715,#4908);
#4234=LINE('',#21721,#4909);
#4235=LINE('',#21731,#4910);
#4236=LINE('',#21737,#4911);
#4237=LINE('',#21747,#4912);
#4238=LINE('',#21753,#4913);
#4239=LINE('',#21760,#4914);
#4240=LINE('',#21766,#4915);
#4241=LINE('',#21772,#4916);
#4242=LINE('',#21778,#4917);
#4243=LINE('',#21784,#4918);
#4244=LINE('',#21790,#4919);
#4245=LINE('',#21803,#4920);
#4246=LINE('',#21807,#4921);
#4247=LINE('',#21819,#4922);
#4248=LINE('',#21823,#4923);
#4249=LINE('',#21835,#4924);
#4250=LINE('',#21839,#4925);
#4251=LINE('',#21851,#4926);
#4252=LINE('',#21855,#4927);
#4253=LINE('',#21872,#4928);
#4254=LINE('',#21878,#4929);
#4255=LINE('',#21882,#4930);
#4256=LINE('',#21888,#4931);
#4257=LINE('',#21893,#4932);
#4258=LINE('',#21908,#4933);
#4259=LINE('',#21917,#4934);
#4260=LINE('',#21921,#4935);
#4261=LINE('',#21925,#4936);
#4262=LINE('',#21928,#4937);
#4263=LINE('',#22064,#4938);
#4264=LINE('',#22317,#4939);
#4265=LINE('',#22359,#4940);
#4266=LINE('',#22364,#4941);
#4267=LINE('',#22373,#4942);
#4268=LINE('',#22378,#4943);
#4269=LINE('',#22436,#4944);
#4270=LINE('',#22442,#4945);
#4271=LINE('',#22448,#4946);
#4272=LINE('',#22454,#4947);
#4273=LINE('',#22460,#4948);
#4274=LINE('',#22466,#4949);
#4275=LINE('',#22472,#4950);
#4276=LINE('',#22478,#4951);
#4277=LINE('',#22483,#4952);
#4278=LINE('',#22485,#4953);
#4279=LINE('',#22487,#4954);
#4280=LINE('',#22488,#4955);
#4281=LINE('',#22492,#4956);
#4282=LINE('',#22494,#4957);
#4283=LINE('',#22496,#4958);
#4284=LINE('',#22497,#4959);
#4285=LINE('',#22499,#4960);
#4286=LINE('',#22500,#4961);
#4287=LINE('',#22505,#4962);
#4288=LINE('',#22511,#4963);
#4289=LINE('',#22515,#4964);
#4290=LINE('',#22517,#4965);
#4291=LINE('',#22519,#4966);
#4292=LINE('',#22521,#4967);
#4293=LINE('',#22524,#4968);
#4294=LINE('',#22527,#4969);
#4295=LINE('',#22529,#4970);
#4296=LINE('',#22530,#4971);
#4297=LINE('',#22533,#4972);
#4298=LINE('',#22535,#4973);
#4299=LINE('',#22536,#4974);
#4300=LINE('',#22538,#4975);
#4301=LINE('',#22540,#4976);
#4302=LINE('',#22544,#4977);
#4303=LINE('',#22546,#4978);
#4304=LINE('',#22551,#4979);
#4305=LINE('',#22553,#4980);
#4306=LINE('',#22555,#4981);
#4307=LINE('',#22556,#4982);
#4308=LINE('',#22559,#4983);
#4309=LINE('',#22561,#4984);
#4310=LINE('',#22562,#4985);
#4311=LINE('',#22565,#4986);
#4312=LINE('',#22567,#4987);
#4313=LINE('',#22568,#4988);
#4314=LINE('',#22570,#4989);
#4315=LINE('',#22571,#4990);
#4316=LINE('',#22578,#4991);
#4317=LINE('',#22580,#4992);
#4318=LINE('',#22582,#4993);
#4319=LINE('',#22583,#4994);
#4320=LINE('',#22586,#4995);
#4321=LINE('',#22588,#4996);
#4322=LINE('',#22589,#4997);
#4323=LINE('',#22592,#4998);
#4324=LINE('',#22594,#4999);
#4325=LINE('',#22595,#5000);
#4326=LINE('',#22597,#5001);
#4327=LINE('',#22598,#5002);
#4328=LINE('',#22605,#5003);
#4329=LINE('',#22607,#5004);
#4330=LINE('',#22609,#5005);
#4331=LINE('',#22610,#5006);
#4332=LINE('',#22613,#5007);
#4333=LINE('',#22615,#5008);
#4334=LINE('',#22616,#5009);
#4335=LINE('',#22619,#5010);
#4336=LINE('',#22621,#5011);
#4337=LINE('',#22622,#5012);
#4338=LINE('',#22624,#5013);
#4339=LINE('',#22625,#5014);
#4340=LINE('',#22633,#5015);
#4341=LINE('',#22640,#5016);
#4342=LINE('',#22646,#5017);
#4343=LINE('',#22652,#5018);
#4344=LINE('',#22665,#5019);
#4345=LINE('',#22668,#5020);
#4346=LINE('',#22673,#5021);
#4347=LINE('',#22681,#5022);
#4348=LINE('',#22687,#5023);
#4349=LINE('',#22696,#5024);
#4350=LINE('',#22702,#5025);
#4351=LINE('',#22711,#5026);
#4352=LINE('',#22717,#5027);
#4353=LINE('',#22726,#5028);
#4354=LINE('',#22732,#5029);
#4355=LINE('',#22741,#5030);
#4356=LINE('',#22748,#5031);
#4357=LINE('',#22754,#5032);
#4358=LINE('',#22760,#5033);
#4359=LINE('',#22773,#5034);
#4360=LINE('',#22776,#5035);
#4361=LINE('',#22781,#5036);
#4362=LINE('',#22789,#5037);
#4363=LINE('',#22795,#5038);
#4364=LINE('',#22804,#5039);
#4365=LINE('',#22810,#5040);
#4366=LINE('',#22819,#5041);
#4367=LINE('',#22825,#5042);
#4368=LINE('',#22836,#5043);
#4369=LINE('',#22840,#5044);
#4370=LINE('',#22844,#5045);
#4371=LINE('',#22851,#5046);
#4372=LINE('',#22855,#5047);
#4373=LINE('',#22859,#5048);
#4374=LINE('',#22864,#5049);
#4375=LINE('',#22866,#5050);
#4376=LINE('',#22868,#5051);
#4377=LINE('',#22869,#5052);
#4378=LINE('',#22872,#5053);
#4379=LINE('',#22874,#5054);
#4380=LINE('',#22875,#5055);
#4381=LINE('',#22878,#5056);
#4382=LINE('',#22880,#5057);
#4383=LINE('',#22881,#5058);
#4384=LINE('',#22884,#5059);
#4385=LINE('',#22886,#5060);
#4386=LINE('',#22887,#5061);
#4387=LINE('',#22890,#5062);
#4388=LINE('',#22892,#5063);
#4389=LINE('',#22893,#5064);
#4390=LINE('',#22895,#5065);
#4391=LINE('',#22896,#5066);
#4392=LINE('',#22976,#5067);
#4393=LINE('',#22982,#5068);
#4394=LINE('',#22988,#5069);
#4395=LINE('',#22993,#5070);
#4396=LINE('',#22995,#5071);
#4397=LINE('',#22997,#5072);
#4398=LINE('',#22998,#5073);
#4399=LINE('',#23001,#5074);
#4400=LINE('',#23003,#5075);
#4401=LINE('',#23004,#5076);
#4402=LINE('',#23007,#5077);
#4403=LINE('',#23009,#5078);
#4404=LINE('',#23010,#5079);
#4405=LINE('',#23012,#5080);
#4406=LINE('',#23013,#5081);
#4407=LINE('',#23021,#5082);
#4408=LINE('',#23027,#5083);
#4409=LINE('',#23033,#5084);
#4410=LINE('',#23038,#5085);
#4411=LINE('',#23040,#5086);
#4412=LINE('',#23042,#5087);
#4413=LINE('',#23043,#5088);
#4414=LINE('',#23046,#5089);
#4415=LINE('',#23048,#5090);
#4416=LINE('',#23049,#5091);
#4417=LINE('',#23052,#5092);
#4418=LINE('',#23054,#5093);
#4419=LINE('',#23055,#5094);
#4420=LINE('',#23057,#5095);
#4421=LINE('',#23058,#5096);
#4422=LINE('',#23066,#5097);
#4423=LINE('',#23072,#5098);
#4424=LINE('',#23078,#5099);
#4425=LINE('',#23083,#5100);
#4426=LINE('',#23085,#5101);
#4427=LINE('',#23087,#5102);
#4428=LINE('',#23088,#5103);
#4429=LINE('',#23091,#5104);
#4430=LINE('',#23093,#5105);
#4431=LINE('',#23094,#5106);
#4432=LINE('',#23097,#5107);
#4433=LINE('',#23099,#5108);
#4434=LINE('',#23100,#5109);
#4435=LINE('',#23102,#5110);
#4436=LINE('',#23103,#5111);
#4437=LINE('',#23111,#5112);
#4438=LINE('',#23116,#5113);
#4439=LINE('',#23118,#5114);
#4440=LINE('',#23120,#5115);
#4441=LINE('',#23121,#5116);
#4442=LINE('',#23124,#5117);
#4443=LINE('',#23126,#5118);
#4444=LINE('',#23127,#5119);
#4445=LINE('',#23130,#5120);
#4446=LINE('',#23132,#5121);
#4447=LINE('',#23133,#5122);
#4448=LINE('',#23135,#5123);
#4449=LINE('',#23136,#5124);
#4450=LINE('',#23144,#5125);
#4451=LINE('',#23154,#5126);
#4452=LINE('',#23160,#5127);
#4453=LINE('',#23167,#5128);
#4454=LINE('',#23173,#5129);
#4455=LINE('',#23182,#5130);
#4456=LINE('',#23188,#5131);
#4457=LINE('',#23199,#5132);
#4458=LINE('',#23201,#5133);
#4459=LINE('',#23202,#5134);
#4460=LINE('',#23205,#5135);
#4461=LINE('',#23207,#5136);
#4462=LINE('',#23208,#5137);
#4463=LINE('',#23213,#5138);
#4464=LINE('',#23214,#5139);
#4465=LINE('',#23216,#5140);
#4466=LINE('',#23217,#5141);
#4467=LINE('',#23227,#5142);
#4468=LINE('',#23234,#5143);
#4469=LINE('',#23241,#5144);
#4470=LINE('',#23248,#5145);
#4471=LINE('',#23255,#5146);
#4472=LINE('',#23260,#5147);
#4473=LINE('',#23267,#5148);
#4474=LINE('',#23270,#5149);
#4475=LINE('',#23273,#5150);
#4476=LINE('',#23275,#5151);
#4477=LINE('',#23276,#5152);
#4478=LINE('',#23282,#5153);
#4479=LINE('',#23284,#5154);
#4480=LINE('',#23285,#5155);
#4481=LINE('',#23294,#5156);
#4482=LINE('',#23299,#5157);
#4483=LINE('',#23306,#5158);
#4484=LINE('',#23308,#5159);
#4485=LINE('',#23310,#5160);
#4486=LINE('',#23311,#5161);
#4487=LINE('',#23314,#5162);
#4488=LINE('',#23316,#5163);
#4489=LINE('',#23317,#5164);
#4490=LINE('',#23320,#5165);
#4491=LINE('',#23322,#5166);
#4492=LINE('',#23323,#5167);
#4493=LINE('',#23326,#5168);
#4494=LINE('',#23328,#5169);
#4495=LINE('',#23329,#5170);
#4496=LINE('',#23332,#5171);
#4497=LINE('',#23334,#5172);
#4498=LINE('',#23335,#5173);
#4499=LINE('',#23337,#5174);
#4500=LINE('',#23338,#5175);
#4501=LINE('',#23350,#5176);
#4502=LINE('',#23354,#5177);
#4503=LINE('',#23358,#5178);
#4504=LINE('',#23365,#5179);
#4505=LINE('',#23367,#5180);
#4506=LINE('',#23384,#5181);
#4507=LINE('',#23389,#5182);
#4508=LINE('',#23393,#5183);
#4509=LINE('',#23397,#5184);
#4510=LINE('',#23400,#5185);
#4511=LINE('',#23405,#5186);
#4512=LINE('',#23406,#5187);
#4513=LINE('',#23409,#5188);
#4514=LINE('',#23413,#5189);
#4515=LINE('',#23416,#5190);
#4516=LINE('',#23425,#5191);
#4517=LINE('',#23434,#5192);
#4518=LINE('',#23440,#5193);
#4519=LINE('',#23449,#5194);
#4520=LINE('',#23455,#5195);
#4521=LINE('',#23464,#5196);
#4522=LINE('',#23470,#5197);
#4523=LINE('',#23479,#5198);
#4524=VECTOR('',#15484,0.165);
#4525=VECTOR('',#15491,0.165);
#4526=VECTOR('',#15498,0.164999999999999);
#4527=VECTOR('',#15505,0.164999999999999);
#4528=VECTOR('',#15512,0.210000000000001);
#4529=VECTOR('',#15519,0.210000000000001);
#4530=VECTOR('',#15526,0.210000000000001);
#4531=VECTOR('',#15533,0.210000000000001);
#4532=VECTOR('',#15540,0.21);
#4533=VECTOR('',#15547,0.21);
#4534=VECTOR('',#15554,0.21);
#4535=VECTOR('',#15561,0.21);
#4536=VECTOR('',#15566,1.);
#4537=VECTOR('',#15567,1.);
#4538=VECTOR('',#15568,1.);
#4539=VECTOR('',#15569,1.);
#4540=VECTOR('',#15572,1.);
#4541=VECTOR('',#15573,1.);
#4542=VECTOR('',#15574,1.);
#4543=VECTOR('',#15577,1.);
#4544=VECTOR('',#15578,1.);
#4545=VECTOR('',#15579,1.);
#4546=VECTOR('',#15582,1.);
#4547=VECTOR('',#15583,1.);
#4548=VECTOR('',#15592,1.);
#4549=VECTOR('',#15593,1.);
#4550=VECTOR('',#15594,1.);
#4551=VECTOR('',#15595,1.);
#4552=VECTOR('',#15598,1.);
#4553=VECTOR('',#15599,1.);
#4554=VECTOR('',#15600,1.);
#4555=VECTOR('',#15603,1.);
#4556=VECTOR('',#15604,1.);
#4557=VECTOR('',#15605,1.);
#4558=VECTOR('',#15608,1.);
#4559=VECTOR('',#15609,1.);
#4560=VECTOR('',#15618,1.);
#4561=VECTOR('',#15619,1.);
#4562=VECTOR('',#15620,1.);
#4563=VECTOR('',#15621,1.);
#4564=VECTOR('',#15624,1.);
#4565=VECTOR('',#15625,1.);
#4566=VECTOR('',#15626,1.);
#4567=VECTOR('',#15629,1.);
#4568=VECTOR('',#15630,1.);
#4569=VECTOR('',#15631,1.);
#4570=VECTOR('',#15634,1.);
#4571=VECTOR('',#15635,1.);
#4572=VECTOR('',#15646,0.165);
#4573=VECTOR('',#15653,0.165);
#4574=VECTOR('',#15660,0.165);
#4575=VECTOR('',#15667,0.605);
#4576=VECTOR('',#15674,0.275);
#4577=VECTOR('',#15681,0.275);
#4578=VECTOR('',#15688,0.275);
#4579=VECTOR('',#15695,0.275);
#4580=VECTOR('',#15700,1.);
#4581=VECTOR('',#15701,1.);
#4582=VECTOR('',#15702,1.);
#4583=VECTOR('',#15703,1.);
#4584=VECTOR('',#15704,1.);
#4585=VECTOR('',#15705,1.);
#4586=VECTOR('',#15706,1.);
#4587=VECTOR('',#15707,1.);
#4588=VECTOR('',#15710,1.);
#4589=VECTOR('',#15711,1.);
#4590=VECTOR('',#15712,1.);
#4591=VECTOR('',#15715,1.);
#4592=VECTOR('',#15716,1.);
#4593=VECTOR('',#15717,1.);
#4594=VECTOR('',#15720,1.);
#4595=VECTOR('',#15723,1.);
#4596=VECTOR('',#15724,1.);
#4597=VECTOR('',#15725,1.);
#4598=VECTOR('',#15726,1.);
#4599=VECTOR('',#15729,1.);
#4600=VECTOR('',#15730,1.);
#4601=VECTOR('',#15733,1.);
#4602=VECTOR('',#15734,1.);
#4603=VECTOR('',#15737,1.);
#4604=VECTOR('',#15748,0.164999999999999);
#4605=VECTOR('',#15755,0.164999999999999);
#4606=VECTOR('',#15762,0.164999999999999);
#4607=VECTOR('',#15769,0.605);
#4608=VECTOR('',#15776,0.274999999999999);
#4609=VECTOR('',#15783,0.274999999999999);
#4610=VECTOR('',#15790,0.275);
#4611=VECTOR('',#15797,0.275);
#4612=VECTOR('',#15802,1.);
#4613=VECTOR('',#15803,1.);
#4614=VECTOR('',#15804,1.);
#4615=VECTOR('',#15805,1.);
#4616=VECTOR('',#15806,1.);
#4617=VECTOR('',#15807,1.);
#4618=VECTOR('',#15808,1.);
#4619=VECTOR('',#15809,1.);
#4620=VECTOR('',#15812,1.);
#4621=VECTOR('',#15813,1.);
#4622=VECTOR('',#15814,1.);
#4623=VECTOR('',#15817,1.);
#4624=VECTOR('',#15818,1.);
#4625=VECTOR('',#15819,1.);
#4626=VECTOR('',#15822,1.);
#4627=VECTOR('',#15825,1.);
#4628=VECTOR('',#15826,1.);
#4629=VECTOR('',#15827,1.);
#4630=VECTOR('',#15828,1.);
#4631=VECTOR('',#15831,1.);
#4632=VECTOR('',#15832,1.);
#4633=VECTOR('',#15835,1.);
#4634=VECTOR('',#15836,1.);
#4635=VECTOR('',#15839,1.);
#4636=VECTOR('',#15850,0.165);
#4637=VECTOR('',#15859,0.225);
#4638=VECTOR('',#15866,0.225);
#4639=VECTOR('',#15873,0.225);
#4640=VECTOR('',#15890,1.5);
#4641=VECTOR('',#15893,0.6);
#4642=VECTOR('',#15900,0.6);
#4643=VECTOR('',#15911,0.605);
#4644=VECTOR('',#15918,0.8);
#4645=VECTOR('',#15931,0.605);
#4646=VECTOR('',#15938,0.8);
#4647=VECTOR('',#15951,0.225);
#4648=VECTOR('',#15958,1.);
#4649=VECTOR('',#15971,0.164999999999999);
#4650=VECTOR('',#15980,0.225000000000001);
#4651=VECTOR('',#15987,0.225000000000001);
#4652=VECTOR('',#15994,0.225000000000001);
#4653=VECTOR('',#16011,1.5);
#4654=VECTOR('',#16014,0.600000000000001);
#4655=VECTOR('',#16021,0.600000000000001);
#4656=VECTOR('',#16032,0.605);
#4657=VECTOR('',#16039,0.800000000000001);
#4658=VECTOR('',#16052,0.605);
#4659=VECTOR('',#16059,0.800000000000001);
#4660=VECTOR('',#16072,0.225000000000001);
#4661=VECTOR('',#16079,1.);
#4662=VECTOR('',#16092,1.);
#4663=VECTOR('',#16095,1.);
#4664=VECTOR('',#16100,0.165);
#4665=VECTOR('',#16105,1.);
#4666=VECTOR('',#16106,1.);
#4667=VECTOR('',#16107,1.);
#4668=VECTOR('',#16112,1.);
#4669=VECTOR('',#16113,1.);
#4670=VECTOR('',#16114,1.);
#4671=VECTOR('',#16115,1.);
#4672=VECTOR('',#16126,0.4);
#4673=VECTOR('',#16137,0.225);
#4674=VECTOR('',#16142,0.4);
#4675=VECTOR('',#16151,0.225);
#4676=VECTOR('',#16156,1.6);
#4677=VECTOR('',#16161,0.605);
#4678=VECTOR('',#16166,0.605);
#4679=VECTOR('',#16169,1.);
#4680=VECTOR('',#16170,1.);
#4681=VECTOR('',#16171,1.);
#4682=VECTOR('',#16174,1.);
#4683=VECTOR('',#16175,1.);
#4684=VECTOR('',#16178,1.);
#4685=VECTOR('',#16179,1.);
#4686=VECTOR('',#16190,0.225);
#4687=VECTOR('',#16197,0.225);
#4688=VECTOR('',#16202,1.);
#4689=VECTOR('',#16205,1.);
#4690=VECTOR('',#16210,1.);
#4691=VECTOR('',#16213,1.);
#4692=VECTOR('',#16234,1.02);
#4693=VECTOR('',#16249,0.35);
#4694=VECTOR('',#16258,0.199999999999999);
#4695=VECTOR('',#16271,0.35);
#4696=VECTOR('',#16280,0.2);
#4697=VECTOR('',#16289,0.225);
#4698=VECTOR('',#16296,0.225);
#4699=VECTOR('',#16301,1.);
#4700=VECTOR('',#16304,1.);
#4701=VECTOR('',#16309,1.);
#4702=VECTOR('',#16312,1.);
#4703=VECTOR('',#16333,1.02);
#4704=VECTOR('',#16350,0.35);
#4705=VECTOR('',#16355,0.199999999999999);
#4706=VECTOR('',#16372,0.35);
#4707=VECTOR('',#16377,0.2);
#4708=VECTOR('',#16388,1.);
#4709=VECTOR('',#16391,1.);
#4710=VECTOR('',#16396,0.165);
#4711=VECTOR('',#16401,1.);
#4712=VECTOR('',#16402,1.);
#4713=VECTOR('',#16403,1.);
#4714=VECTOR('',#16408,1.);
#4715=VECTOR('',#16409,1.);
#4716=VECTOR('',#16410,1.);
#4717=VECTOR('',#16411,1.);
#4718=VECTOR('',#16422,0.4);
#4719=VECTOR('',#16433,0.225);
#4720=VECTOR('',#16438,0.4);
#4721=VECTOR('',#16447,0.225);
#4722=VECTOR('',#16452,1.6);
#4723=VECTOR('',#16457,0.605);
#4724=VECTOR('',#16462,0.605);
#4725=VECTOR('',#16465,1.);
#4726=VECTOR('',#16466,1.);
#4727=VECTOR('',#16467,1.);
#4728=VECTOR('',#16470,1.);
#4729=VECTOR('',#16471,1.);
#4730=VECTOR('',#16474,1.);
#4731=VECTOR('',#16475,1.);
#4732=VECTOR('',#16486,0.225);
#4733=VECTOR('',#16493,0.225);
#4734=VECTOR('',#16498,1.);
#4735=VECTOR('',#16501,1.);
#4736=VECTOR('',#16506,1.);
#4737=VECTOR('',#16509,1.);
#4738=VECTOR('',#16530,1.02);
#4739=VECTOR('',#16545,0.35);
#4740=VECTOR('',#16554,0.199999999999999);
#4741=VECTOR('',#16567,0.35);
#4742=VECTOR('',#16576,0.2);
#4743=VECTOR('',#16585,0.225);
#4744=VECTOR('',#16592,0.225);
#4745=VECTOR('',#16597,1.);
#4746=VECTOR('',#16600,1.);
#4747=VECTOR('',#16605,1.);
#4748=VECTOR('',#16608,1.);
#4749=VECTOR('',#16629,1.02);
#4750=VECTOR('',#16646,0.35);
#4751=VECTOR('',#16651,0.199999999999999);
#4752=VECTOR('',#16668,0.35);
#4753=VECTOR('',#16673,0.2);
#4754=VECTOR('',#16684,0.6);
#4755=VECTOR('',#16697,0.6);
#4756=VECTOR('',#16714,0.4);
#4757=VECTOR('',#16719,0.425);
#4758=VECTOR('',#16724,0.41);
#4759=VECTOR('',#16733,0.26);
#4760=VECTOR('',#16738,0.25);
#4761=VECTOR('',#16743,0.225);
#4762=VECTOR('',#16748,1.);
#4763=VECTOR('',#16749,1.);
#4764=VECTOR('',#16750,1.);
#4765=VECTOR('',#16751,1.);
#4766=VECTOR('',#16754,1.);
#4767=VECTOR('',#16755,1.);
#4768=VECTOR('',#16756,1.);
#4769=VECTOR('',#16759,1.);
#4770=VECTOR('',#16760,1.);
#4771=VECTOR('',#16761,1.);
#4772=VECTOR('',#16764,1.);
#4773=VECTOR('',#16765,1.);
#4774=VECTOR('',#16766,1.);
#4775=VECTOR('',#16769,1.);
#4776=VECTOR('',#16770,1.);
#4777=VECTOR('',#16771,1.);
#4778=VECTOR('',#16774,1.);
#4779=VECTOR('',#16775,1.);
#4780=VECTOR('',#16788,0.164999999999999);
#4781=VECTOR('',#16795,0.164999999999999);
#4782=VECTOR('',#16802,0.164999999999999);
#4783=VECTOR('',#16809,0.164999999999999);
#4784=VECTOR('',#16816,1.6);
#4785=VECTOR('',#16821,1.);
#4786=VECTOR('',#16824,1.);
#4787=VECTOR('',#16829,1.);
#4788=VECTOR('',#16832,1.);
#4789=VECTOR('',#16845,1.);
#4790=VECTOR('',#16846,1.);
#4791=VECTOR('',#16849,0.165);
#4792=VECTOR('',#16854,0.165);
#4793=VECTOR('',#16859,0.165);
#4794=VECTOR('',#16864,0.165);
#4795=VECTOR('',#16869,1.6);
#4796=VECTOR('',#16874,1.);
#4797=VECTOR('',#16879,1.);
#4798=VECTOR('',#16888,0.225);
#4799=VECTOR('',#16895,0.225);
#4800=VECTOR('',#16902,0.225);
#4801=VECTOR('',#16909,0.225);
#4802=VECTOR('',#16916,1.02);
#4803=VECTOR('',#16923,2.2);
#4804=VECTOR('',#16940,0.35);
#4805=VECTOR('',#16949,0.2);
#4806=VECTOR('',#16962,0.35);
#4807=VECTOR('',#16971,0.2);
#4808=VECTOR('',#16984,0.35);
#4809=VECTOR('',#16993,0.2);
#4810=VECTOR('',#17006,0.35);
#4811=VECTOR('',#17015,0.2);
#4812=VECTOR('',#17024,0.225);
#4813=VECTOR('',#17031,0.225);
#4814=VECTOR('',#17038,0.225);
#4815=VECTOR('',#17045,0.225);
#4816=VECTOR('',#17052,1.02);
#4817=VECTOR('',#17059,2.2);
#4818=VECTOR('',#17078,0.35);
#4819=VECTOR('',#17083,0.2);
#4820=VECTOR('',#17100,0.35);
#4821=VECTOR('',#17105,0.2);
#4822=VECTOR('',#17122,0.35);
#4823=VECTOR('',#17127,0.2);
#4824=VECTOR('',#17144,0.35);
#4825=VECTOR('',#17149,0.2);
#4826=VECTOR('',#17160,0.225);
#4827=VECTOR('',#17167,0.225);
#4828=VECTOR('',#17174,0.225);
#4829=VECTOR('',#17181,0.225);
#4830=VECTOR('',#17188,1.02);
#4831=VECTOR('',#17195,2.2);
#4832=VECTOR('',#17212,0.35);
#4833=VECTOR('',#17221,0.199999999999999);
#4834=VECTOR('',#17234,0.35);
#4835=VECTOR('',#17243,0.199999999999999);
#4836=VECTOR('',#17256,0.35);
#4837=VECTOR('',#17265,0.199999999999999);
#4838=VECTOR('',#17278,0.35);
#4839=VECTOR('',#17287,0.199999999999999);
#4840=VECTOR('',#17296,0.225);
#4841=VECTOR('',#17303,0.225);
#4842=VECTOR('',#17310,0.225);
#4843=VECTOR('',#17317,0.225);
#4844=VECTOR('',#17324,1.02);
#4845=VECTOR('',#17331,2.2);
#4846=VECTOR('',#17350,0.35);
#4847=VECTOR('',#17355,0.199999999999999);
#4848=VECTOR('',#17372,0.35);
#4849=VECTOR('',#17377,0.199999999999999);
#4850=VECTOR('',#17394,0.35);
#4851=VECTOR('',#17399,0.199999999999999);
#4852=VECTOR('',#17416,0.35);
#4853=VECTOR('',#17421,0.199999999999999);
#4854=VECTOR('',#17434,0.164999999999999);
#4855=VECTOR('',#17441,0.164999999999999);
#4856=VECTOR('',#17448,0.164999999999999);
#4857=VECTOR('',#17455,0.164999999999999);
#4858=VECTOR('',#17462,1.6);
#4859=VECTOR('',#17467,1.);
#4860=VECTOR('',#17470,1.);
#4861=VECTOR('',#17475,1.);
#4862=VECTOR('',#17476,1.);
#4863=VECTOR('',#17477,1.);
#4864=VECTOR('',#17480,1.);
#4865=VECTOR('',#17497,0.164999999999999);
#4866=VECTOR('',#17502,0.164999999999999);
#4867=VECTOR('',#17507,0.164999999999999);
#4868=VECTOR('',#17512,0.164999999999999);
#4869=VECTOR('',#17517,1.6);
#4870=VECTOR('',#17520,1.);
#4871=VECTOR('',#17525,1.);
#4872=VECTOR('',#17534,0.225000000000001);
#4873=VECTOR('',#17541,0.225000000000001);
#4874=VECTOR('',#17548,0.225000000000001);
#4875=VECTOR('',#17555,0.225000000000001);
#4876=VECTOR('',#17562,1.02);
#4877=VECTOR('',#17569,2.2);
#4878=VECTOR('',#17586,0.350000000000001);
#4879=VECTOR('',#17595,0.199999999999999);
#4880=VECTOR('',#17608,0.350000000000001);
#4881=VECTOR('',#17617,0.199999999999999);
#4882=VECTOR('',#17630,0.350000000000001);
#4883=VECTOR('',#17639,0.199999999999999);
#4884=VECTOR('',#17652,0.350000000000001);
#4885=VECTOR('',#17661,0.199999999999999);
#4886=VECTOR('',#17670,0.225000000000001);
#4887=VECTOR('',#17677,0.225000000000001);
#4888=VECTOR('',#17684,0.225000000000001);
#4889=VECTOR('',#17691,0.225000000000001);
#4890=VECTOR('',#17698,1.02);
#4891=VECTOR('',#17705,2.2);
#4892=VECTOR('',#17724,0.350000000000001);
#4893=VECTOR('',#17729,0.199999999999999);
#4894=VECTOR('',#17746,0.350000000000001);
#4895=VECTOR('',#17751,0.199999999999999);
#4896=VECTOR('',#17768,0.350000000000001);
#4897=VECTOR('',#17773,0.199999999999999);
#4898=VECTOR('',#17790,0.350000000000001);
#4899=VECTOR('',#17795,0.199999999999999);
#4900=VECTOR('',#17806,0.225000000000001);
#4901=VECTOR('',#17813,0.225000000000001);
#4902=VECTOR('',#17820,0.225000000000001);
#4903=VECTOR('',#17827,0.225000000000001);
#4904=VECTOR('',#17834,1.02);
#4905=VECTOR('',#17841,2.2);
#4906=VECTOR('',#17858,0.350000000000001);
#4907=VECTOR('',#17867,0.199999999999999);
#4908=VECTOR('',#17880,0.350000000000001);
#4909=VECTOR('',#17889,0.199999999999999);
#4910=VECTOR('',#17902,0.350000000000001);
#4911=VECTOR('',#17911,0.199999999999999);
#4912=VECTOR('',#17924,0.350000000000001);
#4913=VECTOR('',#17933,0.199999999999999);
#4914=VECTOR('',#17942,0.225000000000001);
#4915=VECTOR('',#17949,0.225000000000001);
#4916=VECTOR('',#17956,0.225000000000001);
#4917=VECTOR('',#17963,0.225000000000001);
#4918=VECTOR('',#17970,1.02);
#4919=VECTOR('',#17977,2.2);
#4920=VECTOR('',#17996,0.350000000000001);
#4921=VECTOR('',#18001,0.199999999999999);
#4922=VECTOR('',#18018,0.350000000000001);
#4923=VECTOR('',#18023,0.199999999999999);
#4924=VECTOR('',#18040,0.350000000000001);
#4925=VECTOR('',#18045,0.199999999999999);
#4926=VECTOR('',#18062,0.350000000000001);
#4927=VECTOR('',#18067,0.199999999999999);
#4928=VECTOR('',#18090,1.070235);
#4929=VECTOR('',#18097,0.6);
#4930=VECTOR('',#18102,0.63);
#4931=VECTOR('',#18111,1.070235);
#4932=VECTOR('',#18118,0.63);
#4933=VECTOR('',#18137,1.129765);
#4934=VECTOR('',#18148,1.57);
#4935=VECTOR('',#18153,1.6);
#4936=VECTOR('',#18158,1.57);
#4937=VECTOR('',#18163,1.129765);
#4938=VECTOR('',#18210,1.123812);
#4939=VECTOR('',#18279,1.076188);
#4940=VECTOR('',#18308,1.119765);
#4941=VECTOR('',#18315,1.085235);
#4942=VECTOR('',#18326,1.119765);
#4943=VECTOR('',#18333,1.085235);
#4944=VECTOR('',#18444,0.164999999999999);
#4945=VECTOR('',#18451,0.164999999999999);
#4946=VECTOR('',#18458,0.164999999999999);
#4947=VECTOR('',#18465,0.605);
#4948=VECTOR('',#18472,0.164999999999999);
#4949=VECTOR('',#18479,0.164999999999999);
#4950=VECTOR('',#18486,0.164999999999999);
#4951=VECTOR('',#18493,0.605);
#4952=VECTOR('',#18498,1.);
#4953=VECTOR('',#18499,1.);
#4954=VECTOR('',#18500,1.);
#4955=VECTOR('',#18501,1.);
#4956=VECTOR('',#18504,1.);
#4957=VECTOR('',#18505,1.);
#4958=VECTOR('',#18506,1.);
#4959=VECTOR('',#18507,1.);
#4960=VECTOR('',#18510,1.);
#4961=VECTOR('',#18511,1.);
#4962=VECTOR('',#18516,1.);
#4963=VECTOR('',#18523,1.);
#4964=VECTOR('',#18528,1.);
#4965=VECTOR('',#18529,1.);
#4966=VECTOR('',#18530,1.);
#4967=VECTOR('',#18531,1.);
#4968=VECTOR('',#18534,1.);
#4969=VECTOR('',#18537,1.);
#4970=VECTOR('',#18538,1.);
#4971=VECTOR('',#18539,1.);
#4972=VECTOR('',#18542,1.);
#4973=VECTOR('',#18543,1.);
#4974=VECTOR('',#18544,1.);
#4975=VECTOR('',#18547,1.);
#4976=VECTOR('',#18550,1.);
#4977=VECTOR('',#18555,1.);
#4978=VECTOR('',#18558,1.);
#4979=VECTOR('',#18563,1.);
#4980=VECTOR('',#18564,1.);
#4981=VECTOR('',#18565,1.);
#4982=VECTOR('',#18566,1.);
#4983=VECTOR('',#18569,1.);
#4984=VECTOR('',#18570,1.);
#4985=VECTOR('',#18571,1.);
#4986=VECTOR('',#18574,1.);
#4987=VECTOR('',#18575,1.);
#4988=VECTOR('',#18576,1.);
#4989=VECTOR('',#18579,1.);
#4990=VECTOR('',#18580,1.);
#4991=VECTOR('',#18589,1.);
#4992=VECTOR('',#18590,1.);
#4993=VECTOR('',#18591,1.);
#4994=VECTOR('',#18592,1.);
#4995=VECTOR('',#18595,1.);
#4996=VECTOR('',#18596,1.);
#4997=VECTOR('',#18597,1.);
#4998=VECTOR('',#18600,1.);
#4999=VECTOR('',#18601,1.);
#5000=VECTOR('',#18602,1.);
#5001=VECTOR('',#18605,1.);
#5002=VECTOR('',#18606,1.);
#5003=VECTOR('',#18615,1.);
#5004=VECTOR('',#18616,1.);
#5005=VECTOR('',#18617,1.);
#5006=VECTOR('',#18618,1.);
#5007=VECTOR('',#18621,1.);
#5008=VECTOR('',#18622,1.);
#5009=VECTOR('',#18623,1.);
#5010=VECTOR('',#18626,1.);
#5011=VECTOR('',#18627,1.);
#5012=VECTOR('',#18628,1.);
#5013=VECTOR('',#18631,1.);
#5014=VECTOR('',#18632,1.);
#5015=VECTOR('',#18643,0.164999999999999);
#5016=VECTOR('',#18652,0.225);
#5017=VECTOR('',#18659,0.225);
#5018=VECTOR('',#18666,0.225);
#5019=VECTOR('',#18683,1.5);
#5020=VECTOR('',#18686,0.6);
#5021=VECTOR('',#18693,0.6);
#5022=VECTOR('',#18704,0.605);
#5023=VECTOR('',#18711,0.800000000000001);
#5024=VECTOR('',#18724,0.605);
#5025=VECTOR('',#18731,0.800000000000001);
#5026=VECTOR('',#18744,0.605);
#5027=VECTOR('',#18751,0.800000000000001);
#5028=VECTOR('',#18764,0.225);
#5029=VECTOR('',#18771,1.);
#5030=VECTOR('',#18784,0.164999999999999);
#5031=VECTOR('',#18793,0.225000000000001);
#5032=VECTOR('',#18800,0.225000000000001);
#5033=VECTOR('',#18807,0.225000000000001);
#5034=VECTOR('',#18824,1.5);
#5035=VECTOR('',#18827,0.600000000000001);
#5036=VECTOR('',#18834,0.600000000000001);
#5037=VECTOR('',#18845,0.605);
#5038=VECTOR('',#18852,0.800000000000001);
#5039=VECTOR('',#18865,0.605);
#5040=VECTOR('',#18872,0.800000000000001);
#5041=VECTOR('',#18885,0.225000000000001);
#5042=VECTOR('',#18892,1.);
#5043=VECTOR('',#18909,0.325);
#5044=VECTOR('',#18914,0.35);
#5045=VECTOR('',#18919,0.335);
#5046=VECTOR('',#18928,0.21);
#5047=VECTOR('',#18933,0.2);
#5048=VECTOR('',#18938,0.18);
#5049=VECTOR('',#18943,1.);
#5050=VECTOR('',#18944,1.);
#5051=VECTOR('',#18945,1.);
#5052=VECTOR('',#18946,1.);
#5053=VECTOR('',#18949,1.);
#5054=VECTOR('',#18950,1.);
#5055=VECTOR('',#18951,1.);
#5056=VECTOR('',#18954,1.);
#5057=VECTOR('',#18955,1.);
#5058=VECTOR('',#18956,1.);
#5059=VECTOR('',#18959,1.);
#5060=VECTOR('',#18960,1.);
#5061=VECTOR('',#18961,1.);
#5062=VECTOR('',#18964,1.);
#5063=VECTOR('',#18965,1.);
#5064=VECTOR('',#18966,1.);
#5065=VECTOR('',#18969,1.);
#5066=VECTOR('',#18970,1.);
#5067=VECTOR('',#19125,0.5);
#5068=VECTOR('',#19132,1.05);
#5069=VECTOR('',#19139,1.05);
#5070=VECTOR('',#19144,1.);
#5071=VECTOR('',#19145,1.);
#5072=VECTOR('',#19146,1.);
#5073=VECTOR('',#19147,1.);
#5074=VECTOR('',#19150,1.);
#5075=VECTOR('',#19151,1.);
#5076=VECTOR('',#19152,1.);
#5077=VECTOR('',#19155,1.);
#5078=VECTOR('',#19156,1.);
#5079=VECTOR('',#19157,1.);
#5080=VECTOR('',#19160,1.);
#5081=VECTOR('',#19161,1.);
#5082=VECTOR('',#19172,0.65);
#5083=VECTOR('',#19179,0.8);
#5084=VECTOR('',#19186,0.8);
#5085=VECTOR('',#19191,1.);
#5086=VECTOR('',#19192,1.);
#5087=VECTOR('',#19193,1.);
#5088=VECTOR('',#19194,1.);
#5089=VECTOR('',#19197,1.);
#5090=VECTOR('',#19198,1.);
#5091=VECTOR('',#19199,1.);
#5092=VECTOR('',#19202,1.);
#5093=VECTOR('',#19203,1.);
#5094=VECTOR('',#19204,1.);
#5095=VECTOR('',#19207,1.);
#5096=VECTOR('',#19208,1.);
#5097=VECTOR('',#19219,0.65);
#5098=VECTOR('',#19226,0.8);
#5099=VECTOR('',#19233,0.8);
#5100=VECTOR('',#19238,1.);
#5101=VECTOR('',#19239,1.);
#5102=VECTOR('',#19240,1.);
#5103=VECTOR('',#19241,1.);
#5104=VECTOR('',#19244,1.);
#5105=VECTOR('',#19245,1.);
#5106=VECTOR('',#19246,1.);
#5107=VECTOR('',#19249,1.);
#5108=VECTOR('',#19250,1.);
#5109=VECTOR('',#19251,1.);
#5110=VECTOR('',#19254,1.);
#5111=VECTOR('',#19255,1.);
#5112=VECTOR('',#19266,0.305);
#5113=VECTOR('',#19271,1.);
#5114=VECTOR('',#19272,1.);
#5115=VECTOR('',#19273,1.);
#5116=VECTOR('',#19274,1.);
#5117=VECTOR('',#19277,1.);
#5118=VECTOR('',#19278,1.);
#5119=VECTOR('',#19279,1.);
#5120=VECTOR('',#19282,1.);
#5121=VECTOR('',#19283,1.);
#5122=VECTOR('',#19284,1.);
#5123=VECTOR('',#19287,1.);
#5124=VECTOR('',#19288,1.);
#5125=VECTOR('',#19299,0.165);
#5126=VECTOR('',#19312,0.5);
#5127=VECTOR('',#19321,0.3);
#5128=VECTOR('',#19330,0.225);
#5129=VECTOR('',#19337,0.6);
#5130=VECTOR('',#19350,0.305);
#5131=VECTOR('',#19357,0.45);
#5132=VECTOR('',#19372,1.);
#5133=VECTOR('',#19373,1.);
#5134=VECTOR('',#19374,1.);
#5135=VECTOR('',#19377,1.);
#5136=VECTOR('',#19378,1.);
#5137=VECTOR('',#19379,1.);
#5138=VECTOR('',#19384,1.);
#5139=VECTOR('',#19385,1.);
#5140=VECTOR('',#19388,1.);
#5141=VECTOR('',#19389,1.);
#5142=VECTOR('',#19402,1.05);
#5143=VECTOR('',#19411,1.);
#5144=VECTOR('',#19420,1.05);
#5145=VECTOR('',#19429,1.);
#5146=VECTOR('',#19438,1.05);
#5147=VECTOR('',#19445,0.9);
#5148=VECTOR('',#19452,1.);
#5149=VECTOR('',#19455,1.);
#5150=VECTOR('',#19458,1.);
#5151=VECTOR('',#19459,1.);
#5152=VECTOR('',#19460,1.);
#5153=VECTOR('',#19467,1.);
#5154=VECTOR('',#19470,1.);
#5155=VECTOR('',#19471,1.);
#5156=VECTOR('',#19482,0.895);
#5157=VECTOR('',#19489,0.605);
#5158=VECTOR('',#19498,1.);
#5159=VECTOR('',#19499,1.);
#5160=VECTOR('',#19500,1.);
#5161=VECTOR('',#19501,1.);
#5162=VECTOR('',#19504,1.);
#5163=VECTOR('',#19505,1.);
#5164=VECTOR('',#19506,1.);
#5165=VECTOR('',#19509,1.);
#5166=VECTOR('',#19510,1.);
#5167=VECTOR('',#19511,1.);
#5168=VECTOR('',#19514,1.);
#5169=VECTOR('',#19515,1.);
#5170=VECTOR('',#19516,1.);
#5171=VECTOR('',#19519,1.);
#5172=VECTOR('',#19520,1.);
#5173=VECTOR('',#19521,1.);
#5174=VECTOR('',#19524,1.);
#5175=VECTOR('',#19525,1.);
#5176=VECTOR('',#19542,0.325);
#5177=VECTOR('',#19547,0.35);
#5178=VECTOR('',#19552,0.335);
#5179=VECTOR('',#19561,0.21);
#5180=VECTOR('',#19564,0.2);
#5181=VECTOR('',#19593,0.605);
#5182=VECTOR('',#19598,1.);
#5183=VECTOR('',#19601,1.);
#5184=VECTOR('',#19606,1.);
#5185=VECTOR('',#19609,1.);
#5186=VECTOR('',#19614,1.);
#5187=VECTOR('',#19615,1.);
#5188=VECTOR('',#19618,0.305);
#5189=VECTOR('',#19623,1.);
#5190=VECTOR('',#19628,1.);
#5191=VECTOR('',#19641,0.6);
#5192=VECTOR('',#19654,0.6);
#5193=VECTOR('',#19661,0.9);
#5194=VECTOR('',#19674,0.6);
#5195=VECTOR('',#19681,0.9);
#5196=VECTOR('',#19694,0.6);
#5197=VECTOR('',#19701,2.);
#5198=VECTOR('',#19714,0.4);
#5199=CIRCLE('',#13680,0.165);
#5200=CIRCLE('',#13681,0.165);
#5201=CIRCLE('',#13683,0.165);
#5202=CIRCLE('',#13684,0.165);
#5203=CIRCLE('',#13686,0.164999999999999);
#5204=CIRCLE('',#13687,0.164999999999999);
#5205=CIRCLE('',#13689,0.164999999999999);
#5206=CIRCLE('',#13690,0.164999999999999);
#5207=CIRCLE('',#13692,0.210000000000001);
#5208=CIRCLE('',#13693,0.210000000000001);
#5209=CIRCLE('',#13695,0.210000000000001);
#5210=CIRCLE('',#13696,0.210000000000001);
#5211=CIRCLE('',#13698,0.210000000000001);
#5212=CIRCLE('',#13699,0.210000000000001);
#5213=CIRCLE('',#13701,0.210000000000001);
#5214=CIRCLE('',#13702,0.210000000000001);
#5215=CIRCLE('',#13704,0.21);
#5216=CIRCLE('',#13705,0.21);
#5217=CIRCLE('',#13707,0.21);
#5218=CIRCLE('',#13708,0.21);
#5219=CIRCLE('',#13710,0.21);
#5220=CIRCLE('',#13711,0.21);
#5221=CIRCLE('',#13713,0.21);
#5222=CIRCLE('',#13714,0.21);
#5223=CIRCLE('',#13737,0.165);
#5224=CIRCLE('',#13738,0.165);
#5225=CIRCLE('',#13740,0.165);
#5226=CIRCLE('',#13741,0.165);
#5227=CIRCLE('',#13743,0.165);
#5228=CIRCLE('',#13744,0.165);
#5229=CIRCLE('',#13746,0.605);
#5230=CIRCLE('',#13747,0.605);
#5231=CIRCLE('',#13749,0.275);
#5232=CIRCLE('',#13750,0.275);
#5233=CIRCLE('',#13752,0.275);
#5234=CIRCLE('',#13753,0.275);
#5235=CIRCLE('',#13755,0.275);
#5236=CIRCLE('',#13756,0.275);
#5237=CIRCLE('',#13758,0.275);
#5238=CIRCLE('',#13759,0.275);
#5239=CIRCLE('',#13772,0.164999999999999);
#5240=CIRCLE('',#13773,0.164999999999999);
#5241=CIRCLE('',#13775,0.164999999999999);
#5242=CIRCLE('',#13776,0.164999999999999);
#5243=CIRCLE('',#13778,0.164999999999999);
#5244=CIRCLE('',#13779,0.164999999999999);
#5245=CIRCLE('',#13781,0.605);
#5246=CIRCLE('',#13782,0.605);
#5247=CIRCLE('',#13784,0.274999999999999);
#5248=CIRCLE('',#13785,0.274999999999999);
#5249=CIRCLE('',#13787,0.274999999999999);
#5250=CIRCLE('',#13788,0.274999999999999);
#5251=CIRCLE('',#13790,0.275);
#5252=CIRCLE('',#13791,0.275);
#5253=CIRCLE('',#13793,0.275);
#5254=CIRCLE('',#13794,0.275);
#5255=CIRCLE('',#13807,0.165);
#5256=CIRCLE('',#13808,0.165);
#5257=CIRCLE('',#13811,0.225);
#5258=CIRCLE('',#13812,0.225);
#5259=CIRCLE('',#13814,0.225);
#5260=CIRCLE('',#13815,0.225);
#5261=CIRCLE('',#13817,0.225);
#5262=CIRCLE('',#13818,0.225);
#5263=CIRCLE('',#13820,1.5);
#5264=CIRCLE('',#13821,0.6);
#5265=CIRCLE('',#13823,1.5);
#5266=CIRCLE('',#13824,0.6);
#5267=CIRCLE('',#13827,0.6);
#5268=CIRCLE('',#13829,0.6);
#5269=CIRCLE('',#13834,0.605);
#5270=CIRCLE('',#13835,0.605);
#5271=CIRCLE('',#13837,0.8);
#5272=CIRCLE('',#13838,0.8);
#5273=CIRCLE('',#13843,0.605);
#5274=CIRCLE('',#13844,0.605);
#5275=CIRCLE('',#13846,0.8);
#5276=CIRCLE('',#13847,0.8);
#5277=CIRCLE('',#13852,0.225);
#5278=CIRCLE('',#13853,0.225);
#5279=CIRCLE('',#13855,1.);
#5280=CIRCLE('',#13856,1.);
#5281=CIRCLE('',#13861,0.164999999999999);
#5282=CIRCLE('',#13862,0.164999999999999);
#5283=CIRCLE('',#13865,0.225000000000001);
#5284=CIRCLE('',#13866,0.225000000000001);
#5285=CIRCLE('',#13868,0.225000000000001);
#5286=CIRCLE('',#13869,0.225000000000001);
#5287=CIRCLE('',#13871,0.225000000000001);
#5288=CIRCLE('',#13872,0.225000000000001);
#5289=CIRCLE('',#13874,1.5);
#5290=CIRCLE('',#13875,0.600000000000001);
#5291=CIRCLE('',#13877,1.5);
#5292=CIRCLE('',#13878,0.600000000000001);
#5293=CIRCLE('',#13881,0.600000000000001);
#5294=CIRCLE('',#13883,0.600000000000001);
#5295=CIRCLE('',#13888,0.605);
#5296=CIRCLE('',#13889,0.605);
#5297=CIRCLE('',#13891,0.800000000000001);
#5298=CIRCLE('',#13892,0.800000000000001);
#5299=CIRCLE('',#13897,0.605);
#5300=CIRCLE('',#13898,0.605);
#5301=CIRCLE('',#13900,0.800000000000001);
#5302=CIRCLE('',#13901,0.800000000000001);
#5303=CIRCLE('',#13906,0.225000000000001);
#5304=CIRCLE('',#13907,0.225000000000001);
#5305=CIRCLE('',#13909,1.);
#5306=CIRCLE('',#13910,1.);
#5307=CIRCLE('',#13915,0.164999999999999);
#5308=CIRCLE('',#13916,0.164999999999999);
#5309=CIRCLE('',#13918,0.165);
#5310=CIRCLE('',#13919,0.165);
#5311=CIRCLE('',#13921,0.4);
#5312=CIRCLE('',#13923,0.605);
#5313=CIRCLE('',#13924,0.605);
#5314=CIRCLE('',#13925,1.6);
#5315=CIRCLE('',#13927,0.4);
#5316=CIRCLE('',#13928,0.4);
#5317=CIRCLE('',#13930,0.225);
#5318=CIRCLE('',#13932,0.225);
#5319=CIRCLE('',#13934,0.4);
#5320=CIRCLE('',#13936,0.225);
#5321=CIRCLE('',#13938,0.225);
#5322=CIRCLE('',#13940,1.6);
#5323=CIRCLE('',#13942,0.605);
#5324=CIRCLE('',#13944,0.605);
#5325=CIRCLE('',#13952,0.225);
#5326=CIRCLE('',#13953,0.225);
#5327=CIRCLE('',#13955,0.225);
#5328=CIRCLE('',#13956,0.225);
#5329=CIRCLE('',#13958,0.61);
#5330=CIRCLE('',#13959,0.61);
#5331=CIRCLE('',#13961,0.61);
#5332=CIRCLE('',#13962,0.61);
#5333=CIRCLE('',#13964,2.1);
#5334=CIRCLE('',#13965,2.1);
#5335=CIRCLE('',#13966,1.02);
#5336=CIRCLE('',#13968,2.1);
#5337=CIRCLE('',#13970,2.1);
#5338=CIRCLE('',#13972,1.02);
#5339=CIRCLE('',#13976,0.35);
#5340=CIRCLE('',#13977,0.199999999999999);
#5341=CIRCLE('',#13979,0.35);
#5342=CIRCLE('',#13982,0.199999999999999);
#5343=CIRCLE('',#13986,0.35);
#5344=CIRCLE('',#13987,0.2);
#5345=CIRCLE('',#13989,0.35);
#5346=CIRCLE('',#13992,0.2);
#5347=CIRCLE('',#13996,0.225);
#5348=CIRCLE('',#13997,0.225);
#5349=CIRCLE('',#13999,0.225);
#5350=CIRCLE('',#14000,0.225);
#5351=CIRCLE('',#14002,0.61);
#5352=CIRCLE('',#14003,0.61);
#5353=CIRCLE('',#14005,0.61);
#5354=CIRCLE('',#14006,0.61);
#5355=CIRCLE('',#14008,2.1);
#5356=CIRCLE('',#14009,2.1);
#5357=CIRCLE('',#14010,1.02);
#5358=CIRCLE('',#14012,2.1);
#5359=CIRCLE('',#14014,2.1);
#5360=CIRCLE('',#14016,1.02);
#5361=CIRCLE('',#14020,0.35);
#5362=CIRCLE('',#14021,0.199999999999999);
#5363=CIRCLE('',#14023,0.35);
#5364=CIRCLE('',#14026,0.199999999999999);
#5365=CIRCLE('',#14030,0.35);
#5366=CIRCLE('',#14031,0.2);
#5367=CIRCLE('',#14033,0.35);
#5368=CIRCLE('',#14036,0.2);
#5369=CIRCLE('',#14040,0.164999999999999);
#5370=CIRCLE('',#14041,0.164999999999999);
#5371=CIRCLE('',#14043,0.165);
#5372=CIRCLE('',#14044,0.165);
#5373=CIRCLE('',#14046,0.4);
#5374=CIRCLE('',#14048,0.605);
#5375=CIRCLE('',#14049,0.605);
#5376=CIRCLE('',#14050,1.6);
#5377=CIRCLE('',#14052,0.4);
#5378=CIRCLE('',#14053,0.4);
#5379=CIRCLE('',#14055,0.225);
#5380=CIRCLE('',#14057,0.225);
#5381=CIRCLE('',#14059,0.4);
#5382=CIRCLE('',#14061,0.225);
#5383=CIRCLE('',#14063,0.225);
#5384=CIRCLE('',#14065,1.6);
#5385=CIRCLE('',#14067,0.605);
#5386=CIRCLE('',#14069,0.605);
#5387=CIRCLE('',#14077,0.225);
#5388=CIRCLE('',#14078,0.225);
#5389=CIRCLE('',#14080,0.225);
#5390=CIRCLE('',#14081,0.225);
#5391=CIRCLE('',#14083,0.61);
#5392=CIRCLE('',#14084,0.61);
#5393=CIRCLE('',#14086,0.61);
#5394=CIRCLE('',#14087,0.61);
#5395=CIRCLE('',#14089,2.1);
#5396=CIRCLE('',#14090,2.1);
#5397=CIRCLE('',#14091,1.02);
#5398=CIRCLE('',#14093,2.1);
#5399=CIRCLE('',#14095,2.1);
#5400=CIRCLE('',#14097,1.02);
#5401=CIRCLE('',#14101,0.35);
#5402=CIRCLE('',#14102,0.199999999999999);
#5403=CIRCLE('',#14104,0.35);
#5404=CIRCLE('',#14107,0.199999999999999);
#5405=CIRCLE('',#14111,0.35);
#5406=CIRCLE('',#14112,0.2);
#5407=CIRCLE('',#14114,0.35);
#5408=CIRCLE('',#14117,0.2);
#5409=CIRCLE('',#14121,0.225);
#5410=CIRCLE('',#14122,0.225);
#5411=CIRCLE('',#14124,0.225);
#5412=CIRCLE('',#14125,0.225);
#5413=CIRCLE('',#14127,0.61);
#5414=CIRCLE('',#14128,0.61);
#5415=CIRCLE('',#14130,0.61);
#5416=CIRCLE('',#14131,0.61);
#5417=CIRCLE('',#14133,2.1);
#5418=CIRCLE('',#14134,2.1);
#5419=CIRCLE('',#14135,1.02);
#5420=CIRCLE('',#14137,2.1);
#5421=CIRCLE('',#14139,2.1);
#5422=CIRCLE('',#14141,1.02);
#5423=CIRCLE('',#14145,0.35);
#5424=CIRCLE('',#14146,0.199999999999999);
#5425=CIRCLE('',#14148,0.35);
#5426=CIRCLE('',#14151,0.199999999999999);
#5427=CIRCLE('',#14155,0.35);
#5428=CIRCLE('',#14156,0.2);
#5429=CIRCLE('',#14158,0.35);
#5430=CIRCLE('',#14161,0.2);
#5431=CIRCLE('',#14165,0.6);
#5432=CIRCLE('',#14166,0.6);
#5433=CIRCLE('',#14171,0.6);
#5434=CIRCLE('',#14172,0.6);
#5435=CIRCLE('',#14177,0.375);
#5436=CIRCLE('',#14179,0.425);
#5437=CIRCLE('',#14181,0.425);
#5438=CIRCLE('',#14183,0.395);
#5439=CIRCLE('',#14185,0.27);
#5440=CIRCLE('',#14187,0.24505);
#5441=CIRCLE('',#14189,0.24505);
#5442=CIRCLE('',#14191,0.2);
#5443=CIRCLE('',#14204,0.164999999999999);
#5444=CIRCLE('',#14205,0.164999999999999);
#5445=CIRCLE('',#14207,0.164999999999999);
#5446=CIRCLE('',#14208,0.164999999999999);
#5447=CIRCLE('',#14210,0.164999999999999);
#5448=CIRCLE('',#14211,0.164999999999999);
#5449=CIRCLE('',#14213,0.164999999999999);
#5450=CIRCLE('',#14214,0.164999999999999);
#5451=CIRCLE('',#14216,1.6);
#5452=CIRCLE('',#14217,1.6);
#5453=CIRCLE('',#14219,2.2);
#5454=CIRCLE('',#14220,2.2);
#5455=CIRCLE('',#14222,2.2);
#5456=CIRCLE('',#14223,1.6);
#5457=CIRCLE('',#14224,0.165);
#5458=CIRCLE('',#14225,0.165);
#5459=CIRCLE('',#14226,0.165);
#5460=CIRCLE('',#14227,0.165);
#5461=CIRCLE('',#14230,0.165);
#5462=CIRCLE('',#14232,0.165);
#5463=CIRCLE('',#14234,0.165);
#5464=CIRCLE('',#14236,0.165);
#5465=CIRCLE('',#14238,1.6);
#5466=CIRCLE('',#14240,2.2);
#5467=CIRCLE('',#14245,0.225);
#5468=CIRCLE('',#14246,0.225);
#5469=CIRCLE('',#14248,0.225);
#5470=CIRCLE('',#14249,0.225);
#5471=CIRCLE('',#14251,0.225);
#5472=CIRCLE('',#14252,0.225);
#5473=CIRCLE('',#14254,0.225);
#5474=CIRCLE('',#14255,0.225);
#5475=CIRCLE('',#14257,1.02);
#5476=CIRCLE('',#14258,1.02);
#5477=CIRCLE('',#14260,2.2);
#5478=CIRCLE('',#14261,2.2);
#5479=CIRCLE('',#14266,0.35);
#5480=CIRCLE('',#14267,0.2);
#5481=CIRCLE('',#14269,0.35);
#5482=CIRCLE('',#14272,0.2);
#5483=CIRCLE('',#14276,0.35);
#5484=CIRCLE('',#14277,0.2);
#5485=CIRCLE('',#14279,0.35);
#5486=CIRCLE('',#14282,0.2);
#5487=CIRCLE('',#14286,0.35);
#5488=CIRCLE('',#14287,0.2);
#5489=CIRCLE('',#14289,0.35);
#5490=CIRCLE('',#14292,0.2);
#5491=CIRCLE('',#14296,0.35);
#5492=CIRCLE('',#14297,0.2);
#5493=CIRCLE('',#14299,0.35);
#5494=CIRCLE('',#14302,0.2);
#5495=CIRCLE('',#14306,0.225);
#5496=CIRCLE('',#14307,0.225);
#5497=CIRCLE('',#14309,0.225);
#5498=CIRCLE('',#14310,0.225);
#5499=CIRCLE('',#14312,0.225);
#5500=CIRCLE('',#14313,0.225);
#5501=CIRCLE('',#14315,0.225);
#5502=CIRCLE('',#14316,0.225);
#5503=CIRCLE('',#14318,1.02);
#5504=CIRCLE('',#14319,1.02);
#5505=CIRCLE('',#14321,2.2);
#5506=CIRCLE('',#14322,2.2);
#5507=CIRCLE('',#14327,0.35);
#5508=CIRCLE('',#14328,0.2);
#5509=CIRCLE('',#14330,0.35);
#5510=CIRCLE('',#14333,0.2);
#5511=CIRCLE('',#14337,0.35);
#5512=CIRCLE('',#14338,0.2);
#5513=CIRCLE('',#14340,0.35);
#5514=CIRCLE('',#14343,0.2);
#5515=CIRCLE('',#14347,0.35);
#5516=CIRCLE('',#14348,0.2);
#5517=CIRCLE('',#14350,0.35);
#5518=CIRCLE('',#14353,0.2);
#5519=CIRCLE('',#14357,0.35);
#5520=CIRCLE('',#14358,0.2);
#5521=CIRCLE('',#14360,0.35);
#5522=CIRCLE('',#14363,0.2);
#5523=CIRCLE('',#14367,0.225);
#5524=CIRCLE('',#14368,0.225);
#5525=CIRCLE('',#14370,0.225);
#5526=CIRCLE('',#14371,0.225);
#5527=CIRCLE('',#14373,0.225);
#5528=CIRCLE('',#14374,0.225);
#5529=CIRCLE('',#14376,0.225);
#5530=CIRCLE('',#14377,0.225);
#5531=CIRCLE('',#14379,1.02);
#5532=CIRCLE('',#14380,1.02);
#5533=CIRCLE('',#14382,2.2);
#5534=CIRCLE('',#14383,2.2);
#5535=CIRCLE('',#14388,0.35);
#5536=CIRCLE('',#14389,0.199999999999999);
#5537=CIRCLE('',#14391,0.35);
#5538=CIRCLE('',#14394,0.199999999999999);
#5539=CIRCLE('',#14398,0.35);
#5540=CIRCLE('',#14399,0.199999999999999);
#5541=CIRCLE('',#14401,0.35);
#5542=CIRCLE('',#14404,0.199999999999999);
#5543=CIRCLE('',#14408,0.35);
#5544=CIRCLE('',#14409,0.199999999999999);
#5545=CIRCLE('',#14411,0.35);
#5546=CIRCLE('',#14414,0.199999999999999);
#5547=CIRCLE('',#14418,0.35);
#5548=CIRCLE('',#14419,0.199999999999999);
#5549=CIRCLE('',#14421,0.35);
#5550=CIRCLE('',#14424,0.199999999999999);
#5551=CIRCLE('',#14428,0.225);
#5552=CIRCLE('',#14429,0.225);
#5553=CIRCLE('',#14431,0.225);
#5554=CIRCLE('',#14432,0.225);
#5555=CIRCLE('',#14434,0.225);
#5556=CIRCLE('',#14435,0.225);
#5557=CIRCLE('',#14437,0.225);
#5558=CIRCLE('',#14438,0.225);
#5559=CIRCLE('',#14440,1.02);
#5560=CIRCLE('',#14441,1.02);
#5561=CIRCLE('',#14443,2.2);
#5562=CIRCLE('',#14444,2.2);
#5563=CIRCLE('',#14449,0.35);
#5564=CIRCLE('',#14450,0.199999999999999);
#5565=CIRCLE('',#14452,0.35);
#5566=CIRCLE('',#14455,0.199999999999999);
#5567=CIRCLE('',#14459,0.35);
#5568=CIRCLE('',#14460,0.199999999999999);
#5569=CIRCLE('',#14462,0.35);
#5570=CIRCLE('',#14465,0.199999999999999);
#5571=CIRCLE('',#14469,0.35);
#5572=CIRCLE('',#14470,0.199999999999999);
#5573=CIRCLE('',#14472,0.35);
#5574=CIRCLE('',#14475,0.199999999999999);
#5575=CIRCLE('',#14479,0.35);
#5576=CIRCLE('',#14480,0.199999999999999);
#5577=CIRCLE('',#14482,0.35);
#5578=CIRCLE('',#14485,0.199999999999999);
#5579=CIRCLE('',#14490,0.164999999999999);
#5580=CIRCLE('',#14491,0.164999999999999);
#5581=CIRCLE('',#14493,0.164999999999999);
#5582=CIRCLE('',#14494,0.164999999999999);
#5583=CIRCLE('',#14496,0.164999999999999);
#5584=CIRCLE('',#14497,0.164999999999999);
#5585=CIRCLE('',#14499,0.164999999999999);
#5586=CIRCLE('',#14500,0.164999999999999);
#5587=CIRCLE('',#14502,1.6);
#5588=CIRCLE('',#14503,1.6);
#5589=CIRCLE('',#14505,2.2);
#5590=CIRCLE('',#14506,2.2);
#5591=CIRCLE('',#14509,2.2);
#5592=CIRCLE('',#14510,1.6);
#5593=CIRCLE('',#14511,0.164999999999999);
#5594=CIRCLE('',#14512,0.164999999999999);
#5595=CIRCLE('',#14513,0.164999999999999);
#5596=CIRCLE('',#14514,0.164999999999999);
#5597=CIRCLE('',#14516,0.164999999999999);
#5598=CIRCLE('',#14518,0.164999999999999);
#5599=CIRCLE('',#14520,0.164999999999999);
#5600=CIRCLE('',#14522,0.164999999999999);
#5601=CIRCLE('',#14524,1.6);
#5602=CIRCLE('',#14526,2.2);
#5603=CIRCLE('',#14531,0.225000000000001);
#5604=CIRCLE('',#14532,0.225000000000001);
#5605=CIRCLE('',#14534,0.225000000000001);
#5606=CIRCLE('',#14535,0.225000000000001);
#5607=CIRCLE('',#14537,0.225000000000001);
#5608=CIRCLE('',#14538,0.225000000000001);
#5609=CIRCLE('',#14540,0.225000000000001);
#5610=CIRCLE('',#14541,0.225000000000001);
#5611=CIRCLE('',#14543,1.02);
#5612=CIRCLE('',#14544,1.02);
#5613=CIRCLE('',#14546,2.2);
#5614=CIRCLE('',#14547,2.2);
#5615=CIRCLE('',#14552,0.350000000000001);
#5616=CIRCLE('',#14553,0.199999999999999);
#5617=CIRCLE('',#14555,0.350000000000001);
#5618=CIRCLE('',#14558,0.199999999999999);
#5619=CIRCLE('',#14562,0.350000000000001);
#5620=CIRCLE('',#14563,0.199999999999999);
#5621=CIRCLE('',#14565,0.350000000000001);
#5622=CIRCLE('',#14568,0.199999999999999);
#5623=CIRCLE('',#14572,0.350000000000001);
#5624=CIRCLE('',#14573,0.199999999999999);
#5625=CIRCLE('',#14575,0.350000000000001);
#5626=CIRCLE('',#14578,0.199999999999999);
#5627=CIRCLE('',#14582,0.350000000000001);
#5628=CIRCLE('',#14583,0.199999999999999);
#5629=CIRCLE('',#14585,0.350000000000001);
#5630=CIRCLE('',#14588,0.199999999999999);
#5631=CIRCLE('',#14592,0.225000000000001);
#5632=CIRCLE('',#14593,0.225000000000001);
#5633=CIRCLE('',#14595,0.225000000000001);
#5634=CIRCLE('',#14596,0.225000000000001);
#5635=CIRCLE('',#14598,0.225000000000001);
#5636=CIRCLE('',#14599,0.225000000000001);
#5637=CIRCLE('',#14601,0.225000000000001);
#5638=CIRCLE('',#14602,0.225000000000001);
#5639=CIRCLE('',#14604,1.02);
#5640=CIRCLE('',#14605,1.02);
#5641=CIRCLE('',#14607,2.2);
#5642=CIRCLE('',#14608,2.2);
#5643=CIRCLE('',#14613,0.350000000000001);
#5644=CIRCLE('',#14614,0.199999999999999);
#5645=CIRCLE('',#14616,0.350000000000001);
#5646=CIRCLE('',#14619,0.199999999999999);
#5647=CIRCLE('',#14623,0.350000000000001);
#5648=CIRCLE('',#14624,0.199999999999999);
#5649=CIRCLE('',#14626,0.350000000000001);
#5650=CIRCLE('',#14629,0.199999999999999);
#5651=CIRCLE('',#14633,0.350000000000001);
#5652=CIRCLE('',#14634,0.199999999999999);
#5653=CIRCLE('',#14636,0.350000000000001);
#5654=CIRCLE('',#14639,0.199999999999999);
#5655=CIRCLE('',#14643,0.350000000000001);
#5656=CIRCLE('',#14644,0.199999999999999);
#5657=CIRCLE('',#14646,0.350000000000001);
#5658=CIRCLE('',#14649,0.199999999999999);
#5659=CIRCLE('',#14653,0.225000000000001);
#5660=CIRCLE('',#14654,0.225000000000001);
#5661=CIRCLE('',#14656,0.225000000000001);
#5662=CIRCLE('',#14657,0.225000000000001);
#5663=CIRCLE('',#14659,0.225000000000001);
#5664=CIRCLE('',#14660,0.225000000000001);
#5665=CIRCLE('',#14662,0.225000000000001);
#5666=CIRCLE('',#14663,0.225000000000001);
#5667=CIRCLE('',#14665,1.02);
#5668=CIRCLE('',#14666,1.02);
#5669=CIRCLE('',#14668,2.2);
#5670=CIRCLE('',#14669,2.2);
#5671=CIRCLE('',#14674,0.350000000000001);
#5672=CIRCLE('',#14675,0.199999999999999);
#5673=CIRCLE('',#14677,0.350000000000001);
#5674=CIRCLE('',#14680,0.199999999999999);
#5675=CIRCLE('',#14684,0.350000000000001);
#5676=CIRCLE('',#14685,0.199999999999999);
#5677=CIRCLE('',#14687,0.350000000000001);
#5678=CIRCLE('',#14690,0.199999999999999);
#5679=CIRCLE('',#14694,0.350000000000001);
#5680=CIRCLE('',#14695,0.199999999999999);
#5681=CIRCLE('',#14697,0.350000000000001);
#5682=CIRCLE('',#14700,0.199999999999999);
#5683=CIRCLE('',#14704,0.350000000000001);
#5684=CIRCLE('',#14705,0.199999999999999);
#5685=CIRCLE('',#14707,0.350000000000001);
#5686=CIRCLE('',#14710,0.199999999999999);
#5687=CIRCLE('',#14714,0.225000000000001);
#5688=CIRCLE('',#14715,0.225000000000001);
#5689=CIRCLE('',#14717,0.225000000000001);
#5690=CIRCLE('',#14718,0.225000000000001);
#5691=CIRCLE('',#14720,0.225000000000001);
#5692=CIRCLE('',#14721,0.225000000000001);
#5693=CIRCLE('',#14723,0.225000000000001);
#5694=CIRCLE('',#14724,0.225000000000001);
#5695=CIRCLE('',#14726,1.02);
#5696=CIRCLE('',#14727,1.02);
#5697=CIRCLE('',#14729,2.2);
#5698=CIRCLE('',#14730,2.2);
#5699=CIRCLE('',#14735,0.350000000000001);
#5700=CIRCLE('',#14736,0.199999999999999);
#5701=CIRCLE('',#14738,0.350000000000001);
#5702=CIRCLE('',#14741,0.199999999999999);
#5703=CIRCLE('',#14745,0.350000000000001);
#5704=CIRCLE('',#14746,0.199999999999999);
#5705=CIRCLE('',#14748,0.350000000000001);
#5706=CIRCLE('',#14751,0.199999999999999);
#5707=CIRCLE('',#14755,0.350000000000001);
#5708=CIRCLE('',#14756,0.199999999999999);
#5709=CIRCLE('',#14758,0.350000000000001);
#5710=CIRCLE('',#14761,0.199999999999999);
#5711=CIRCLE('',#14765,0.350000000000001);
#5712=CIRCLE('',#14766,0.199999999999999);
#5713=CIRCLE('',#14768,0.350000000000001);
#5714=CIRCLE('',#14771,0.199999999999999);
#5715=CIRCLE('',#14776,1.070235);
#5716=CIRCLE('',#14777,1.070235);
#5717=CIRCLE('',#14778,0.309556);
#5718=CIRCLE('',#14779,1.070235);
#5719=CIRCLE('',#14780,1.070235);
#5720=CIRCLE('',#14782,1.070235);
#5721=CIRCLE('',#14784,0.6);
#5722=CIRCLE('',#14785,0.6);
#5723=CIRCLE('',#14787,0.66);
#5724=CIRCLE('',#14790,1.070235);
#5725=CIRCLE('',#14792,0.66);
#5726=CIRCLE('',#14796,1.129765);
#5727=CIRCLE('',#14797,1.129765);
#5728=CIRCLE('',#14798,0.309556);
#5729=CIRCLE('',#14799,1.129765);
#5730=CIRCLE('',#14800,1.129765);
#5731=CIRCLE('',#14802,1.129765);
#5732=CIRCLE('',#14804,1.54);
#5733=CIRCLE('',#14805,1.129765);
#5734=CIRCLE('',#14807,1.6);
#5735=CIRCLE('',#14809,1.6);
#5736=CIRCLE('',#14811,1.54);
#5737=CIRCLE('',#14816,0.29765);
#5738=CIRCLE('',#14818,0.29765);
#5739=CIRCLE('',#14820,0.29765);
#5740=CIRCLE('',#14822,0.29765);
#5741=CIRCLE('',#14824,0.29765);
#5742=CIRCLE('',#14826,0.29765);
#5743=CIRCLE('',#14828,0.29765);
#5744=CIRCLE('',#14831,0.303778037777585);
#5745=CIRCLE('',#14832,0.303778037777585);
#5746=CIRCLE('',#14834,1.123812);
#5747=CIRCLE('',#14835,1.123812);
#5748=CIRCLE('',#14836,1.123812);
#5749=CIRCLE('',#14837,1.123812);
#5750=CIRCLE('',#14838,1.123812);
#5751=CIRCLE('',#14839,1.123812);
#5752=CIRCLE('',#14840,1.123812);
#5753=CIRCLE('',#14841,1.123812);
#5754=CIRCLE('',#14842,1.123812);
#5755=CIRCLE('',#14844,1.076188);
#5756=CIRCLE('',#14845,0.303778037777585);
#5757=CIRCLE('',#14847,0.303778037777585);
#5758=CIRCLE('',#14849,1.076188);
#5759=CIRCLE('',#14850,0.303778037777585);
#5760=CIRCLE('',#14852,0.303778037777585);
#5761=CIRCLE('',#14854,1.076188);
#5762=CIRCLE('',#14855,1.076188);
#5763=CIRCLE('',#14856,0.303778037777585);
#5764=CIRCLE('',#14858,0.303778037777585);
#5765=CIRCLE('',#14860,1.076188);
#5766=CIRCLE('',#14861,0.303778037777585);
#5767=CIRCLE('',#14863,0.303778037777585);
#5768=CIRCLE('',#14865,1.076188);
#5769=CIRCLE('',#14866,0.303778037777585);
#5770=CIRCLE('',#14868,0.303778037777585);
#5771=CIRCLE('',#14870,1.076188);
#5772=CIRCLE('',#14871,1.076188);
#5773=CIRCLE('',#14872,1.076188);
#5774=CIRCLE('',#14874,0.303778037777585);
#5775=CIRCLE('',#14876,0.303778037777585);
#5776=CIRCLE('',#14881,1.119765);
#5777=CIRCLE('',#14882,1.085235);
#5778=CIRCLE('',#14884,1.119765);
#5779=CIRCLE('',#14886,1.085235);
#5780=CIRCLE('',#14889,1.119765);
#5781=CIRCLE('',#14890,1.085235);
#5782=CIRCLE('',#14892,1.119765);
#5783=CIRCLE('',#14894,1.085235);
#5784=CIRCLE('',#14950,0.164999999999999);
#5785=CIRCLE('',#14951,0.164999999999999);
#5786=CIRCLE('',#14953,0.164999999999999);
#5787=CIRCLE('',#14954,0.164999999999999);
#5788=CIRCLE('',#14956,0.164999999999999);
#5789=CIRCLE('',#14957,0.164999999999999);
#5790=CIRCLE('',#14959,0.605);
#5791=CIRCLE('',#14960,0.605);
#5792=CIRCLE('',#14962,0.164999999999999);
#5793=CIRCLE('',#14963,0.164999999999999);
#5794=CIRCLE('',#14965,0.164999999999999);
#5795=CIRCLE('',#14966,0.164999999999999);
#5796=CIRCLE('',#14968,0.164999999999999);
#5797=CIRCLE('',#14969,0.164999999999999);
#5798=CIRCLE('',#14971,0.605);
#5799=CIRCLE('',#14972,0.605);
#5800=CIRCLE('',#14977,1.8);
#5801=CIRCLE('',#14978,1.8);
#5802=CIRCLE('',#14980,1.8);
#5803=CIRCLE('',#14981,1.8);
#5804=CIRCLE('',#14983,1.8);
#5805=CIRCLE('',#14989,1.8);
#5806=CIRCLE('',#15014,0.164999999999999);
#5807=CIRCLE('',#15015,0.164999999999999);
#5808=CIRCLE('',#15018,0.225);
#5809=CIRCLE('',#15019,0.225);
#5810=CIRCLE('',#15021,0.225);
#5811=CIRCLE('',#15022,0.225);
#5812=CIRCLE('',#15024,0.225);
#5813=CIRCLE('',#15025,0.225);
#5814=CIRCLE('',#15027,1.5);
#5815=CIRCLE('',#15028,0.6);
#5816=CIRCLE('',#15030,1.5);
#5817=CIRCLE('',#15031,0.6);
#5818=CIRCLE('',#15034,0.6);
#5819=CIRCLE('',#15036,0.6);
#5820=CIRCLE('',#15041,0.605);
#5821=CIRCLE('',#15042,0.605);
#5822=CIRCLE('',#15044,0.800000000000001);
#5823=CIRCLE('',#15045,0.800000000000001);
#5824=CIRCLE('',#15050,0.605);
#5825=CIRCLE('',#15051,0.605);
#5826=CIRCLE('',#15053,0.800000000000001);
#5827=CIRCLE('',#15054,0.800000000000001);
#5828=CIRCLE('',#15059,0.605);
#5829=CIRCLE('',#15060,0.605);
#5830=CIRCLE('',#15062,0.800000000000001);
#5831=CIRCLE('',#15063,0.800000000000001);
#5832=CIRCLE('',#15068,0.225);
#5833=CIRCLE('',#15069,0.225);
#5834=CIRCLE('',#15071,1.);
#5835=CIRCLE('',#15072,1.);
#5836=CIRCLE('',#15077,0.164999999999999);
#5837=CIRCLE('',#15078,0.164999999999999);
#5838=CIRCLE('',#15081,0.225000000000001);
#5839=CIRCLE('',#15082,0.225000000000001);
#5840=CIRCLE('',#15084,0.225000000000001);
#5841=CIRCLE('',#15085,0.225000000000001);
#5842=CIRCLE('',#15087,0.225000000000001);
#5843=CIRCLE('',#15088,0.225000000000001);
#5844=CIRCLE('',#15090,1.5);
#5845=CIRCLE('',#15091,0.600000000000001);
#5846=CIRCLE('',#15093,1.5);
#5847=CIRCLE('',#15094,0.600000000000001);
#5848=CIRCLE('',#15097,0.600000000000001);
#5849=CIRCLE('',#15099,0.600000000000001);
#5850=CIRCLE('',#15104,0.605);
#5851=CIRCLE('',#15105,0.605);
#5852=CIRCLE('',#15107,0.800000000000001);
#5853=CIRCLE('',#15108,0.800000000000001);
#5854=CIRCLE('',#15113,0.605);
#5855=CIRCLE('',#15114,0.605);
#5856=CIRCLE('',#15116,0.800000000000001);
#5857=CIRCLE('',#15117,0.800000000000001);
#5858=CIRCLE('',#15122,0.225000000000001);
#5859=CIRCLE('',#15123,0.225000000000001);
#5860=CIRCLE('',#15125,1.);
#5861=CIRCLE('',#15126,1.);
#5862=CIRCLE('',#15131,0.3);
#5863=CIRCLE('',#15133,0.35);
#5864=CIRCLE('',#15135,0.35);
#5865=CIRCLE('',#15137,0.32);
#5866=CIRCLE('',#15139,0.22);
#5867=CIRCLE('',#15141,0.1954);
#5868=CIRCLE('',#15143,0.1954);
#5869=CIRCLE('',#15145,0.16);
#5870=CIRCLE('',#15229,0.5);
#5871=CIRCLE('',#15230,0.5);
#5872=CIRCLE('',#15232,1.05);
#5873=CIRCLE('',#15233,1.05);
#5874=CIRCLE('',#15235,1.05);
#5875=CIRCLE('',#15236,1.05);
#5876=CIRCLE('',#15245,0.65);
#5877=CIRCLE('',#15246,0.65);
#5878=CIRCLE('',#15248,0.8);
#5879=CIRCLE('',#15249,0.8);
#5880=CIRCLE('',#15251,0.8);
#5881=CIRCLE('',#15252,0.8);
#5882=CIRCLE('',#15261,0.65);
#5883=CIRCLE('',#15262,0.65);
#5884=CIRCLE('',#15264,0.8);
#5885=CIRCLE('',#15265,0.8);
#5886=CIRCLE('',#15267,0.8);
#5887=CIRCLE('',#15268,0.8);
#5888=CIRCLE('',#15277,0.305);
#5889=CIRCLE('',#15278,0.305);
#5890=CIRCLE('',#15287,0.165);
#5891=CIRCLE('',#15288,0.165);
#5892=CIRCLE('',#15291,0.5);
#5893=CIRCLE('',#15292,0.3);
#5894=CIRCLE('',#15294,0.5);
#5895=CIRCLE('',#15297,0.3);
#5896=CIRCLE('',#15301,0.225);
#5897=CIRCLE('',#15302,0.225);
#5898=CIRCLE('',#15304,0.6);
#5899=CIRCLE('',#15305,0.6);
#5900=CIRCLE('',#15310,0.305);
#5901=CIRCLE('',#15311,0.305);
#5902=CIRCLE('',#15313,0.45);
#5903=CIRCLE('',#15314,0.45);
#5904=CIRCLE('',#15320,0.9);
#5905=CIRCLE('',#15323,0.9);
#5906=CIRCLE('',#15327,1.05);
#5907=CIRCLE('',#15328,0.9);
#5908=CIRCLE('',#15330,1.05);
#5909=CIRCLE('',#15332,1.);
#5910=CIRCLE('',#15334,1.);
#5911=CIRCLE('',#15336,1.05);
#5912=CIRCLE('',#15338,1.05);
#5913=CIRCLE('',#15340,1.);
#5914=CIRCLE('',#15342,1.);
#5915=CIRCLE('',#15344,1.05);
#5916=CIRCLE('',#15346,1.05);
#5917=CIRCLE('',#15348,0.9);
#5918=CIRCLE('',#15352,0.895);
#5919=CIRCLE('',#15353,0.605);
#5920=CIRCLE('',#15356,0.895);
#5921=CIRCLE('',#15357,0.605);
#5922=CIRCLE('',#15360,0.895);
#5923=CIRCLE('',#15361,0.605);
#5924=CIRCLE('',#15363,0.895);
#5925=CIRCLE('',#15365,0.605);
#5926=CIRCLE('',#15379,0.1954);
#5927=CIRCLE('',#15381,0.3);
#5928=CIRCLE('',#15383,0.35);
#5929=CIRCLE('',#15385,0.35);
#5930=CIRCLE('',#15387,0.32);
#5931=CIRCLE('',#15389,0.22);
#5932=CIRCLE('',#15391,0.1954);
#5933=CIRCLE('',#15406,0.605);
#5934=CIRCLE('',#15407,0.605);
#5935=CIRCLE('',#15409,1.1);
#5936=CIRCLE('',#15410,1.1);
#5937=CIRCLE('',#15412,0.8);
#5938=CIRCLE('',#15413,0.305);
#5939=CIRCLE('',#15416,0.305);
#5940=CIRCLE('',#15418,0.8);
#5941=CIRCLE('',#15425,0.6);
#5942=CIRCLE('',#15426,0.6);
#5943=CIRCLE('',#15431,0.6);
#5944=CIRCLE('',#15432,0.6);
#5945=CIRCLE('',#15434,0.9);
#5946=CIRCLE('',#15435,0.9);
#5947=CIRCLE('',#15440,0.6);
#5948=CIRCLE('',#15441,0.6);
#5949=CIRCLE('',#15443,0.9);
#5950=CIRCLE('',#15444,0.9);
#5951=CIRCLE('',#15449,0.6);
#5952=CIRCLE('',#15450,0.6);
#5953=CIRCLE('',#15452,2.);
#5954=CIRCLE('',#15453,2.);
#5955=CIRCLE('',#15458,0.4);
#5956=CIRCLE('',#15459,0.4);
#5957=VERTEX_POINT('',#19749);
#5958=VERTEX_POINT('',#19751);
#5959=VERTEX_POINT('',#19755);
#5960=VERTEX_POINT('',#19757);
#5961=VERTEX_POINT('',#19761);
#5962=VERTEX_POINT('',#19763);
#5963=VERTEX_POINT('',#19767);
#5964=VERTEX_POINT('',#19769);
#5965=VERTEX_POINT('',#19773);
#5966=VERTEX_POINT('',#19775);
#5967=VERTEX_POINT('',#19779);
#5968=VERTEX_POINT('',#19781);
#5969=VERTEX_POINT('',#19785);
#5970=VERTEX_POINT('',#19787);
#5971=VERTEX_POINT('',#19791);
#5972=VERTEX_POINT('',#19793);
#5973=VERTEX_POINT('',#19797);
#5974=VERTEX_POINT('',#19799);
#5975=VERTEX_POINT('',#19803);
#5976=VERTEX_POINT('',#19805);
#5977=VERTEX_POINT('',#19809);
#5978=VERTEX_POINT('',#19811);
#5979=VERTEX_POINT('',#19815);
#5980=VERTEX_POINT('',#19817);
#5981=VERTEX_POINT('',#19821);
#5982=VERTEX_POINT('',#19822);
#5983=VERTEX_POINT('',#19824);
#5984=VERTEX_POINT('',#19826);
#5985=VERTEX_POINT('',#19830);
#5986=VERTEX_POINT('',#19832);
#5987=VERTEX_POINT('',#19836);
#5988=VERTEX_POINT('',#19838);
#5989=VERTEX_POINT('',#19848);
#5990=VERTEX_POINT('',#19849);
#5991=VERTEX_POINT('',#19851);
#5992=VERTEX_POINT('',#19853);
#5993=VERTEX_POINT('',#19857);
#5994=VERTEX_POINT('',#19859);
#5995=VERTEX_POINT('',#19863);
#5996=VERTEX_POINT('',#19865);
#5997=VERTEX_POINT('',#19875);
#5998=VERTEX_POINT('',#19876);
#5999=VERTEX_POINT('',#19878);
#6000=VERTEX_POINT('',#19880);
#6001=VERTEX_POINT('',#19884);
#6002=VERTEX_POINT('',#19886);
#6003=VERTEX_POINT('',#19890);
#6004=VERTEX_POINT('',#19892);
#6005=VERTEX_POINT('',#19902);
#6006=VERTEX_POINT('',#19904);
#6007=VERTEX_POINT('',#19908);
#6008=VERTEX_POINT('',#19910);
#6009=VERTEX_POINT('',#19914);
#6010=VERTEX_POINT('',#19916);
#6011=VERTEX_POINT('',#19920);
#6012=VERTEX_POINT('',#19922);
#6013=VERTEX_POINT('',#19926);
#6014=VERTEX_POINT('',#19928);
#6015=VERTEX_POINT('',#19932);
#6016=VERTEX_POINT('',#19934);
#6017=VERTEX_POINT('',#19938);
#6018=VERTEX_POINT('',#19940);
#6019=VERTEX_POINT('',#19944);
#6020=VERTEX_POINT('',#19946);
#6021=VERTEX_POINT('',#19950);
#6022=VERTEX_POINT('',#19951);
#6023=VERTEX_POINT('',#19953);
#6024=VERTEX_POINT('',#19955);
#6025=VERTEX_POINT('',#19957);
#6026=VERTEX_POINT('',#19959);
#6027=VERTEX_POINT('',#19961);
#6028=VERTEX_POINT('',#19963);
#6029=VERTEX_POINT('',#19967);
#6030=VERTEX_POINT('',#19969);
#6031=VERTEX_POINT('',#19973);
#6032=VERTEX_POINT('',#19975);
#6033=VERTEX_POINT('',#19981);
#6034=VERTEX_POINT('',#19983);
#6035=VERTEX_POINT('',#19988);
#6036=VERTEX_POINT('',#19992);
#6037=VERTEX_POINT('',#20001);
#6038=VERTEX_POINT('',#20003);
#6039=VERTEX_POINT('',#20007);
#6040=VERTEX_POINT('',#20009);
#6041=VERTEX_POINT('',#20013);
#6042=VERTEX_POINT('',#20015);
#6043=VERTEX_POINT('',#20019);
#6044=VERTEX_POINT('',#20021);
#6045=VERTEX_POINT('',#20025);
#6046=VERTEX_POINT('',#20027);
#6047=VERTEX_POINT('',#20031);
#6048=VERTEX_POINT('',#20033);
#6049=VERTEX_POINT('',#20037);
#6050=VERTEX_POINT('',#20039);
#6051=VERTEX_POINT('',#20043);
#6052=VERTEX_POINT('',#20045);
#6053=VERTEX_POINT('',#20049);
#6054=VERTEX_POINT('',#20050);
#6055=VERTEX_POINT('',#20052);
#6056=VERTEX_POINT('',#20054);
#6057=VERTEX_POINT('',#20056);
#6058=VERTEX_POINT('',#20058);
#6059=VERTEX_POINT('',#20060);
#6060=VERTEX_POINT('',#20062);
#6061=VERTEX_POINT('',#20066);
#6062=VERTEX_POINT('',#20068);
#6063=VERTEX_POINT('',#20072);
#6064=VERTEX_POINT('',#20074);
#6065=VERTEX_POINT('',#20080);
#6066=VERTEX_POINT('',#20082);
#6067=VERTEX_POINT('',#20087);
#6068=VERTEX_POINT('',#20091);
#6069=VERTEX_POINT('',#20100);
#6070=VERTEX_POINT('',#20102);
#6071=VERTEX_POINT('',#20107);
#6072=VERTEX_POINT('',#20109);
#6073=VERTEX_POINT('',#20113);
#6074=VERTEX_POINT('',#20115);
#6075=VERTEX_POINT('',#20119);
#6076=VERTEX_POINT('',#20121);
#6077=VERTEX_POINT('',#20125);
#6078=VERTEX_POINT('',#20127);
#6079=VERTEX_POINT('',#20130);
#6080=VERTEX_POINT('',#20132);
#6081=VERTEX_POINT('',#20137);
#6082=VERTEX_POINT('',#20141);
#6083=VERTEX_POINT('',#20148);
#6084=VERTEX_POINT('',#20150);
#6085=VERTEX_POINT('',#20154);
#6086=VERTEX_POINT('',#20156);
#6087=VERTEX_POINT('',#20163);
#6088=VERTEX_POINT('',#20165);
#6089=VERTEX_POINT('',#20169);
#6090=VERTEX_POINT('',#20171);
#6091=VERTEX_POINT('',#20178);
#6092=VERTEX_POINT('',#20180);
#6093=VERTEX_POINT('',#20184);
#6094=VERTEX_POINT('',#20186);
#6095=VERTEX_POINT('',#20193);
#6096=VERTEX_POINT('',#20195);
#6097=VERTEX_POINT('',#20200);
#6098=VERTEX_POINT('',#20202);
#6099=VERTEX_POINT('',#20206);
#6100=VERTEX_POINT('',#20208);
#6101=VERTEX_POINT('',#20212);
#6102=VERTEX_POINT('',#20214);
#6103=VERTEX_POINT('',#20218);
#6104=VERTEX_POINT('',#20220);
#6105=VERTEX_POINT('',#20223);
#6106=VERTEX_POINT('',#20225);
#6107=VERTEX_POINT('',#20230);
#6108=VERTEX_POINT('',#20234);
#6109=VERTEX_POINT('',#20241);
#6110=VERTEX_POINT('',#20243);
#6111=VERTEX_POINT('',#20247);
#6112=VERTEX_POINT('',#20249);
#6113=VERTEX_POINT('',#20256);
#6114=VERTEX_POINT('',#20258);
#6115=VERTEX_POINT('',#20262);
#6116=VERTEX_POINT('',#20264);
#6117=VERTEX_POINT('',#20271);
#6118=VERTEX_POINT('',#20273);
#6119=VERTEX_POINT('',#20277);
#6120=VERTEX_POINT('',#20279);
#6121=VERTEX_POINT('',#20286);
#6122=VERTEX_POINT('',#20287);
#6123=VERTEX_POINT('',#20289);
#6124=VERTEX_POINT('',#20291);
#6125=VERTEX_POINT('',#20295);
#6126=VERTEX_POINT('',#20297);
#6127=VERTEX_POINT('',#20301);
#6128=VERTEX_POINT('',#20303);
#6129=VERTEX_POINT('',#20306);
#6130=VERTEX_POINT('',#20309);
#6131=VERTEX_POINT('',#20311);
#6132=VERTEX_POINT('',#20313);
#6133=VERTEX_POINT('',#20316);
#6134=VERTEX_POINT('',#20318);
#6135=VERTEX_POINT('',#20320);
#6136=VERTEX_POINT('',#20323);
#6137=VERTEX_POINT('',#20325);
#6138=VERTEX_POINT('',#20329);
#6139=VERTEX_POINT('',#20332);
#6140=VERTEX_POINT('',#20336);
#6141=VERTEX_POINT('',#20340);
#6142=VERTEX_POINT('',#20343);
#6143=VERTEX_POINT('',#20347);
#6144=VERTEX_POINT('',#20351);
#6145=VERTEX_POINT('',#20355);
#6146=VERTEX_POINT('',#20359);
#6147=VERTEX_POINT('',#20361);
#6148=VERTEX_POINT('',#20365);
#6149=VERTEX_POINT('',#20375);
#6150=VERTEX_POINT('',#20377);
#6151=VERTEX_POINT('',#20381);
#6152=VERTEX_POINT('',#20383);
#6153=VERTEX_POINT('',#20387);
#6154=VERTEX_POINT('',#20388);
#6155=VERTEX_POINT('',#20390);
#6156=VERTEX_POINT('',#20392);
#6157=VERTEX_POINT('',#20396);
#6158=VERTEX_POINT('',#20397);
#6159=VERTEX_POINT('',#20399);
#6160=VERTEX_POINT('',#20401);
#6161=VERTEX_POINT('',#20407);
#6162=VERTEX_POINT('',#20414);
#6163=VERTEX_POINT('',#20420);
#6164=VERTEX_POINT('',#20422);
#6165=VERTEX_POINT('',#20425);
#6166=VERTEX_POINT('',#20430);
#6167=VERTEX_POINT('',#20436);
#6168=VERTEX_POINT('',#20438);
#6169=VERTEX_POINT('',#20441);
#6170=VERTEX_POINT('',#20446);
#6171=VERTEX_POINT('',#20452);
#6172=VERTEX_POINT('',#20454);
#6173=VERTEX_POINT('',#20458);
#6174=VERTEX_POINT('',#20460);
#6175=VERTEX_POINT('',#20464);
#6176=VERTEX_POINT('',#20465);
#6177=VERTEX_POINT('',#20467);
#6178=VERTEX_POINT('',#20469);
#6179=VERTEX_POINT('',#20473);
#6180=VERTEX_POINT('',#20474);
#6181=VERTEX_POINT('',#20476);
#6182=VERTEX_POINT('',#20478);
#6183=VERTEX_POINT('',#20484);
#6184=VERTEX_POINT('',#20491);
#6185=VERTEX_POINT('',#20497);
#6186=VERTEX_POINT('',#20499);
#6187=VERTEX_POINT('',#20502);
#6188=VERTEX_POINT('',#20507);
#6189=VERTEX_POINT('',#20513);
#6190=VERTEX_POINT('',#20515);
#6191=VERTEX_POINT('',#20518);
#6192=VERTEX_POINT('',#20523);
#6193=VERTEX_POINT('',#20529);
#6194=VERTEX_POINT('',#20530);
#6195=VERTEX_POINT('',#20532);
#6196=VERTEX_POINT('',#20534);
#6197=VERTEX_POINT('',#20538);
#6198=VERTEX_POINT('',#20540);
#6199=VERTEX_POINT('',#20544);
#6200=VERTEX_POINT('',#20546);
#6201=VERTEX_POINT('',#20549);
#6202=VERTEX_POINT('',#20552);
#6203=VERTEX_POINT('',#20554);
#6204=VERTEX_POINT('',#20556);
#6205=VERTEX_POINT('',#20559);
#6206=VERTEX_POINT('',#20561);
#6207=VERTEX_POINT('',#20563);
#6208=VERTEX_POINT('',#20566);
#6209=VERTEX_POINT('',#20568);
#6210=VERTEX_POINT('',#20572);
#6211=VERTEX_POINT('',#20575);
#6212=VERTEX_POINT('',#20579);
#6213=VERTEX_POINT('',#20583);
#6214=VERTEX_POINT('',#20586);
#6215=VERTEX_POINT('',#20590);
#6216=VERTEX_POINT('',#20594);
#6217=VERTEX_POINT('',#20598);
#6218=VERTEX_POINT('',#20602);
#6219=VERTEX_POINT('',#20604);
#6220=VERTEX_POINT('',#20608);
#6221=VERTEX_POINT('',#20618);
#6222=VERTEX_POINT('',#20620);
#6223=VERTEX_POINT('',#20624);
#6224=VERTEX_POINT('',#20626);
#6225=VERTEX_POINT('',#20630);
#6226=VERTEX_POINT('',#20631);
#6227=VERTEX_POINT('',#20633);
#6228=VERTEX_POINT('',#20635);
#6229=VERTEX_POINT('',#20639);
#6230=VERTEX_POINT('',#20640);
#6231=VERTEX_POINT('',#20642);
#6232=VERTEX_POINT('',#20644);
#6233=VERTEX_POINT('',#20650);
#6234=VERTEX_POINT('',#20657);
#6235=VERTEX_POINT('',#20663);
#6236=VERTEX_POINT('',#20665);
#6237=VERTEX_POINT('',#20668);
#6238=VERTEX_POINT('',#20673);
#6239=VERTEX_POINT('',#20679);
#6240=VERTEX_POINT('',#20681);
#6241=VERTEX_POINT('',#20684);
#6242=VERTEX_POINT('',#20689);
#6243=VERTEX_POINT('',#20695);
#6244=VERTEX_POINT('',#20697);
#6245=VERTEX_POINT('',#20701);
#6246=VERTEX_POINT('',#20703);
#6247=VERTEX_POINT('',#20707);
#6248=VERTEX_POINT('',#20708);
#6249=VERTEX_POINT('',#20710);
#6250=VERTEX_POINT('',#20712);
#6251=VERTEX_POINT('',#20716);
#6252=VERTEX_POINT('',#20717);
#6253=VERTEX_POINT('',#20719);
#6254=VERTEX_POINT('',#20721);
#6255=VERTEX_POINT('',#20727);
#6256=VERTEX_POINT('',#20734);
#6257=VERTEX_POINT('',#20740);
#6258=VERTEX_POINT('',#20742);
#6259=VERTEX_POINT('',#20745);
#6260=VERTEX_POINT('',#20750);
#6261=VERTEX_POINT('',#20756);
#6262=VERTEX_POINT('',#20758);
#6263=VERTEX_POINT('',#20761);
#6264=VERTEX_POINT('',#20766);
#6265=VERTEX_POINT('',#20772);
#6266=VERTEX_POINT('',#20774);
#6267=VERTEX_POINT('',#20781);
#6268=VERTEX_POINT('',#20783);
#6269=VERTEX_POINT('',#20790);
#6270=VERTEX_POINT('',#20793);
#6271=VERTEX_POINT('',#20797);
#6272=VERTEX_POINT('',#20801);
#6273=VERTEX_POINT('',#20805);
#6274=VERTEX_POINT('',#20808);
#6275=VERTEX_POINT('',#20812);
#6276=VERTEX_POINT('',#20816);
#6277=VERTEX_POINT('',#20821);
#6278=VERTEX_POINT('',#20822);
#6279=VERTEX_POINT('',#20824);
#6280=VERTEX_POINT('',#20826);
#6281=VERTEX_POINT('',#20830);
#6282=VERTEX_POINT('',#20832);
#6283=VERTEX_POINT('',#20836);
#6284=VERTEX_POINT('',#20838);
#6285=VERTEX_POINT('',#20842);
#6286=VERTEX_POINT('',#20844);
#6287=VERTEX_POINT('',#20848);
#6288=VERTEX_POINT('',#20850);
#6289=VERTEX_POINT('',#20861);
#6290=VERTEX_POINT('',#20863);
#6291=VERTEX_POINT('',#20867);
#6292=VERTEX_POINT('',#20869);
#6293=VERTEX_POINT('',#20873);
#6294=VERTEX_POINT('',#20875);
#6295=VERTEX_POINT('',#20879);
#6296=VERTEX_POINT('',#20881);
#6297=VERTEX_POINT('',#20885);
#6298=VERTEX_POINT('',#20887);
#6299=VERTEX_POINT('',#20891);
#6300=VERTEX_POINT('',#20892);
#6301=VERTEX_POINT('',#20894);
#6302=VERTEX_POINT('',#20896);
#6303=VERTEX_POINT('',#20900);
#6304=VERTEX_POINT('',#20902);
#6305=VERTEX_POINT('',#20905);
#6306=VERTEX_POINT('',#20907);
#6307=VERTEX_POINT('',#20909);
#6308=VERTEX_POINT('',#20911);
#6309=VERTEX_POINT('',#20913);
#6310=VERTEX_POINT('',#20916);
#6311=VERTEX_POINT('',#20920);
#6312=VERTEX_POINT('',#20924);
#6313=VERTEX_POINT('',#20928);
#6314=VERTEX_POINT('',#20932);
#6315=VERTEX_POINT('',#20936);
#6316=VERTEX_POINT('',#20940);
#6317=VERTEX_POINT('',#20948);
#6318=VERTEX_POINT('',#20950);
#6319=VERTEX_POINT('',#20954);
#6320=VERTEX_POINT('',#20956);
#6321=VERTEX_POINT('',#20960);
#6322=VERTEX_POINT('',#20962);
#6323=VERTEX_POINT('',#20966);
#6324=VERTEX_POINT('',#20968);
#6325=VERTEX_POINT('',#20972);
#6326=VERTEX_POINT('',#20974);
#6327=VERTEX_POINT('',#20978);
#6328=VERTEX_POINT('',#20980);
#6329=VERTEX_POINT('',#20987);
#6330=VERTEX_POINT('',#20989);
#6331=VERTEX_POINT('',#20992);
#6332=VERTEX_POINT('',#20997);
#6333=VERTEX_POINT('',#21003);
#6334=VERTEX_POINT('',#21005);
#6335=VERTEX_POINT('',#21008);
#6336=VERTEX_POINT('',#21013);
#6337=VERTEX_POINT('',#21019);
#6338=VERTEX_POINT('',#21021);
#6339=VERTEX_POINT('',#21024);
#6340=VERTEX_POINT('',#21029);
#6341=VERTEX_POINT('',#21035);
#6342=VERTEX_POINT('',#21037);
#6343=VERTEX_POINT('',#21040);
#6344=VERTEX_POINT('',#21045);
#6345=VERTEX_POINT('',#21051);
#6346=VERTEX_POINT('',#21053);
#6347=VERTEX_POINT('',#21057);
#6348=VERTEX_POINT('',#21059);
#6349=VERTEX_POINT('',#21063);
#6350=VERTEX_POINT('',#21065);
#6351=VERTEX_POINT('',#21069);
#6352=VERTEX_POINT('',#21071);
#6353=VERTEX_POINT('',#21075);
#6354=VERTEX_POINT('',#21077);
#6355=VERTEX_POINT('',#21081);
#6356=VERTEX_POINT('',#21083);
#6357=VERTEX_POINT('',#21090);
#6358=VERTEX_POINT('',#21092);
#6359=VERTEX_POINT('',#21095);
#6360=VERTEX_POINT('',#21100);
#6361=VERTEX_POINT('',#21106);
#6362=VERTEX_POINT('',#21108);
#6363=VERTEX_POINT('',#21111);
#6364=VERTEX_POINT('',#21116);
#6365=VERTEX_POINT('',#21122);
#6366=VERTEX_POINT('',#21124);
#6367=VERTEX_POINT('',#21127);
#6368=VERTEX_POINT('',#21132);
#6369=VERTEX_POINT('',#21138);
#6370=VERTEX_POINT('',#21140);
#6371=VERTEX_POINT('',#21143);
#6372=VERTEX_POINT('',#21148);
#6373=VERTEX_POINT('',#21154);
#6374=VERTEX_POINT('',#21156);
#6375=VERTEX_POINT('',#21160);
#6376=VERTEX_POINT('',#21162);
#6377=VERTEX_POINT('',#21166);
#6378=VERTEX_POINT('',#21168);
#6379=VERTEX_POINT('',#21172);
#6380=VERTEX_POINT('',#21174);
#6381=VERTEX_POINT('',#21178);
#6382=VERTEX_POINT('',#21180);
#6383=VERTEX_POINT('',#21184);
#6384=VERTEX_POINT('',#21186);
#6385=VERTEX_POINT('',#21193);
#6386=VERTEX_POINT('',#21195);
#6387=VERTEX_POINT('',#21198);
#6388=VERTEX_POINT('',#21203);
#6389=VERTEX_POINT('',#21209);
#6390=VERTEX_POINT('',#21211);
#6391=VERTEX_POINT('',#21214);
#6392=VERTEX_POINT('',#21219);
#6393=VERTEX_POINT('',#21225);
#6394=VERTEX_POINT('',#21227);
#6395=VERTEX_POINT('',#21230);
#6396=VERTEX_POINT('',#21235);
#6397=VERTEX_POINT('',#21241);
#6398=VERTEX_POINT('',#21243);
#6399=VERTEX_POINT('',#21246);
#6400=VERTEX_POINT('',#21251);
#6401=VERTEX_POINT('',#21257);
#6402=VERTEX_POINT('',#21259);
#6403=VERTEX_POINT('',#21263);
#6404=VERTEX_POINT('',#21265);
#6405=VERTEX_POINT('',#21269);
#6406=VERTEX_POINT('',#21271);
#6407=VERTEX_POINT('',#21275);
#6408=VERTEX_POINT('',#21277);
#6409=VERTEX_POINT('',#21281);
#6410=VERTEX_POINT('',#21283);
#6411=VERTEX_POINT('',#21287);
#6412=VERTEX_POINT('',#21289);
#6413=VERTEX_POINT('',#21296);
#6414=VERTEX_POINT('',#21298);
#6415=VERTEX_POINT('',#21301);
#6416=VERTEX_POINT('',#21306);
#6417=VERTEX_POINT('',#21312);
#6418=VERTEX_POINT('',#21314);
#6419=VERTEX_POINT('',#21317);
#6420=VERTEX_POINT('',#21322);
#6421=VERTEX_POINT('',#21328);
#6422=VERTEX_POINT('',#21330);
#6423=VERTEX_POINT('',#21333);
#6424=VERTEX_POINT('',#21338);
#6425=VERTEX_POINT('',#21344);
#6426=VERTEX_POINT('',#21346);
#6427=VERTEX_POINT('',#21349);
#6428=VERTEX_POINT('',#21354);
#6429=VERTEX_POINT('',#21361);
#6430=VERTEX_POINT('',#21363);
#6431=VERTEX_POINT('',#21367);
#6432=VERTEX_POINT('',#21369);
#6433=VERTEX_POINT('',#21373);
#6434=VERTEX_POINT('',#21375);
#6435=VERTEX_POINT('',#21379);
#6436=VERTEX_POINT('',#21381);
#6437=VERTEX_POINT('',#21385);
#6438=VERTEX_POINT('',#21387);
#6439=VERTEX_POINT('',#21391);
#6440=VERTEX_POINT('',#21392);
#6441=VERTEX_POINT('',#21394);
#6442=VERTEX_POINT('',#21396);
#6443=VERTEX_POINT('',#21400);
#6444=VERTEX_POINT('',#21402);
#6445=VERTEX_POINT('',#21406);
#6446=VERTEX_POINT('',#21409);
#6447=VERTEX_POINT('',#21411);
#6448=VERTEX_POINT('',#21413);
#6449=VERTEX_POINT('',#21415);
#6450=VERTEX_POINT('',#21417);
#6451=VERTEX_POINT('',#21420);
#6452=VERTEX_POINT('',#21424);
#6453=VERTEX_POINT('',#21428);
#6454=VERTEX_POINT('',#21432);
#6455=VERTEX_POINT('',#21436);
#6456=VERTEX_POINT('',#21440);
#6457=VERTEX_POINT('',#21448);
#6458=VERTEX_POINT('',#21450);
#6459=VERTEX_POINT('',#21454);
#6460=VERTEX_POINT('',#21456);
#6461=VERTEX_POINT('',#21460);
#6462=VERTEX_POINT('',#21462);
#6463=VERTEX_POINT('',#21466);
#6464=VERTEX_POINT('',#21468);
#6465=VERTEX_POINT('',#21472);
#6466=VERTEX_POINT('',#21474);
#6467=VERTEX_POINT('',#21478);
#6468=VERTEX_POINT('',#21480);
#6469=VERTEX_POINT('',#21487);
#6470=VERTEX_POINT('',#21489);
#6471=VERTEX_POINT('',#21492);
#6472=VERTEX_POINT('',#21497);
#6473=VERTEX_POINT('',#21503);
#6474=VERTEX_POINT('',#21505);
#6475=VERTEX_POINT('',#21508);
#6476=VERTEX_POINT('',#21513);
#6477=VERTEX_POINT('',#21519);
#6478=VERTEX_POINT('',#21521);
#6479=VERTEX_POINT('',#21524);
#6480=VERTEX_POINT('',#21529);
#6481=VERTEX_POINT('',#21535);
#6482=VERTEX_POINT('',#21537);
#6483=VERTEX_POINT('',#21540);
#6484=VERTEX_POINT('',#21545);
#6485=VERTEX_POINT('',#21551);
#6486=VERTEX_POINT('',#21553);
#6487=VERTEX_POINT('',#21557);
#6488=VERTEX_POINT('',#21559);
#6489=VERTEX_POINT('',#21563);
#6490=VERTEX_POINT('',#21565);
#6491=VERTEX_POINT('',#21569);
#6492=VERTEX_POINT('',#21571);
#6493=VERTEX_POINT('',#21575);
#6494=VERTEX_POINT('',#21577);
#6495=VERTEX_POINT('',#21581);
#6496=VERTEX_POINT('',#21583);
#6497=VERTEX_POINT('',#21590);
#6498=VERTEX_POINT('',#21592);
#6499=VERTEX_POINT('',#21595);
#6500=VERTEX_POINT('',#21600);
#6501=VERTEX_POINT('',#21606);
#6502=VERTEX_POINT('',#21608);
#6503=VERTEX_POINT('',#21611);
#6504=VERTEX_POINT('',#21616);
#6505=VERTEX_POINT('',#21622);
#6506=VERTEX_POINT('',#21624);
#6507=VERTEX_POINT('',#21627);
#6508=VERTEX_POINT('',#21632);
#6509=VERTEX_POINT('',#21638);
#6510=VERTEX_POINT('',#21640);
#6511=VERTEX_POINT('',#21643);
#6512=VERTEX_POINT('',#21648);
#6513=VERTEX_POINT('',#21654);
#6514=VERTEX_POINT('',#21656);
#6515=VERTEX_POINT('',#21660);
#6516=VERTEX_POINT('',#21662);
#6517=VERTEX_POINT('',#21666);
#6518=VERTEX_POINT('',#21668);
#6519=VERTEX_POINT('',#21672);
#6520=VERTEX_POINT('',#21674);
#6521=VERTEX_POINT('',#21678);
#6522=VERTEX_POINT('',#21680);
#6523=VERTEX_POINT('',#21684);
#6524=VERTEX_POINT('',#21686);
#6525=VERTEX_POINT('',#21693);
#6526=VERTEX_POINT('',#21695);
#6527=VERTEX_POINT('',#21698);
#6528=VERTEX_POINT('',#21703);
#6529=VERTEX_POINT('',#21709);
#6530=VERTEX_POINT('',#21711);
#6531=VERTEX_POINT('',#21714);
#6532=VERTEX_POINT('',#21719);
#6533=VERTEX_POINT('',#21725);
#6534=VERTEX_POINT('',#21727);
#6535=VERTEX_POINT('',#21730);
#6536=VERTEX_POINT('',#21735);
#6537=VERTEX_POINT('',#21741);
#6538=VERTEX_POINT('',#21743);
#6539=VERTEX_POINT('',#21746);
#6540=VERTEX_POINT('',#21751);
#6541=VERTEX_POINT('',#21757);
#6542=VERTEX_POINT('',#21759);
#6543=VERTEX_POINT('',#21763);
#6544=VERTEX_POINT('',#21765);
#6545=VERTEX_POINT('',#21769);
#6546=VERTEX_POINT('',#21771);
#6547=VERTEX_POINT('',#21775);
#6548=VERTEX_POINT('',#21777);
#6549=VERTEX_POINT('',#21781);
#6550=VERTEX_POINT('',#21783);
#6551=VERTEX_POINT('',#21787);
#6552=VERTEX_POINT('',#21789);
#6553=VERTEX_POINT('',#21796);
#6554=VERTEX_POINT('',#21798);
#6555=VERTEX_POINT('',#21801);
#6556=VERTEX_POINT('',#21806);
#6557=VERTEX_POINT('',#21812);
#6558=VERTEX_POINT('',#21814);
#6559=VERTEX_POINT('',#21817);
#6560=VERTEX_POINT('',#21822);
#6561=VERTEX_POINT('',#21828);
#6562=VERTEX_POINT('',#21830);
#6563=VERTEX_POINT('',#21833);
#6564=VERTEX_POINT('',#21838);
#6565=VERTEX_POINT('',#21844);
#6566=VERTEX_POINT('',#21846);
#6567=VERTEX_POINT('',#21849);
#6568=VERTEX_POINT('',#21854);
#6569=VERTEX_POINT('',#21861);
#6570=VERTEX_POINT('',#21862);
#6571=VERTEX_POINT('',#21865);
#6572=VERTEX_POINT('',#21867);
#6573=VERTEX_POINT('',#21871);
#6574=VERTEX_POINT('',#21875);
#6575=VERTEX_POINT('',#21877);
#6576=VERTEX_POINT('',#21881);
#6577=VERTEX_POINT('',#21886);
#6578=VERTEX_POINT('',#21890);
#6579=VERTEX_POINT('',#21896);
#6580=VERTEX_POINT('',#21897);
#6581=VERTEX_POINT('',#21900);
#6582=VERTEX_POINT('',#21902);
#6583=VERTEX_POINT('',#21906);
#6584=VERTEX_POINT('',#21910);
#6585=VERTEX_POINT('',#21912);
#6586=VERTEX_POINT('',#21915);
#6587=VERTEX_POINT('',#21919);
#6588=VERTEX_POINT('',#21923);
#6589=VERTEX_POINT('',#21931);
#6590=VERTEX_POINT('',#21932);
#6591=VERTEX_POINT('',#21935);
#6592=VERTEX_POINT('',#21936);
#6593=VERTEX_POINT('',#21939);
#6594=VERTEX_POINT('',#21940);
#6595=VERTEX_POINT('',#21943);
#6596=VERTEX_POINT('',#21944);
#6597=VERTEX_POINT('',#21947);
#6598=VERTEX_POINT('',#21948);
#6599=VERTEX_POINT('',#21951);
#6600=VERTEX_POINT('',#21952);
#6601=VERTEX_POINT('',#21955);
#6602=VERTEX_POINT('',#21956);
#6603=VERTEX_POINT('',#21960);
#6604=VERTEX_POINT('',#21961);
#6605=VERTEX_POINT('',#21984);
#6606=VERTEX_POINT('',#21986);
#6607=VERTEX_POINT('',#22011);
#6608=VERTEX_POINT('',#22013);
#6609=VERTEX_POINT('',#22036);
#6610=VERTEX_POINT('',#22038);
#6611=VERTEX_POINT('',#22061);
#6612=VERTEX_POINT('',#22063);
#6613=VERTEX_POINT('',#22066);
#6614=VERTEX_POINT('',#22068);
#6615=VERTEX_POINT('',#22091);
#6616=VERTEX_POINT('',#22093);
#6617=VERTEX_POINT('',#22116);
#6618=VERTEX_POINT('',#22118);
#6619=VERTEX_POINT('',#22141);
#6620=VERTEX_POINT('',#22143);
#6621=VERTEX_POINT('',#22168);
#6622=VERTEX_POINT('',#22172);
#6623=VERTEX_POINT('',#22197);
#6624=VERTEX_POINT('',#22201);
#6625=VERTEX_POINT('',#22226);
#6626=VERTEX_POINT('',#22228);
#6627=VERTEX_POINT('',#22232);
#6628=VERTEX_POINT('',#22257);
#6629=VERTEX_POINT('',#22261);
#6630=VERTEX_POINT('',#22286);
#6631=VERTEX_POINT('',#22290);
#6632=VERTEX_POINT('',#22315);
#6633=VERTEX_POINT('',#22318);
#6634=VERTEX_POINT('',#22320);
#6635=VERTEX_POINT('',#22352);
#6636=VERTEX_POINT('',#22354);
#6637=VERTEX_POINT('',#22357);
#6638=VERTEX_POINT('',#22361);
#6639=VERTEX_POINT('',#22366);
#6640=VERTEX_POINT('',#22368);
#6641=VERTEX_POINT('',#22371);
#6642=VERTEX_POINT('',#22375);
#6643=VERTEX_POINT('',#22433);
#6644=VERTEX_POINT('',#22435);
#6645=VERTEX_POINT('',#22439);
#6646=VERTEX_POINT('',#22441);
#6647=VERTEX_POINT('',#22445);
#6648=VERTEX_POINT('',#22447);
#6649=VERTEX_POINT('',#22451);
#6650=VERTEX_POINT('',#22453);
#6651=VERTEX_POINT('',#22457);
#6652=VERTEX_POINT('',#22459);
#6653=VERTEX_POINT('',#22463);
#6654=VERTEX_POINT('',#22465);
#6655=VERTEX_POINT('',#22469);
#6656=VERTEX_POINT('',#22471);
#6657=VERTEX_POINT('',#22475);
#6658=VERTEX_POINT('',#22477);
#6659=VERTEX_POINT('',#22481);
#6660=VERTEX_POINT('',#22482);
#6661=VERTEX_POINT('',#22484);
#6662=VERTEX_POINT('',#22486);
#6663=VERTEX_POINT('',#22490);
#6664=VERTEX_POINT('',#22491);
#6665=VERTEX_POINT('',#22493);
#6666=VERTEX_POINT('',#22495);
#6667=VERTEX_POINT('',#22502);
#6668=VERTEX_POINT('',#22504);
#6669=VERTEX_POINT('',#22508);
#6670=VERTEX_POINT('',#22510);
#6671=VERTEX_POINT('',#22514);
#6672=VERTEX_POINT('',#22516);
#6673=VERTEX_POINT('',#22518);
#6674=VERTEX_POINT('',#22520);
#6675=VERTEX_POINT('',#22522);
#6676=VERTEX_POINT('',#22526);
#6677=VERTEX_POINT('',#22528);
#6678=VERTEX_POINT('',#22532);
#6679=VERTEX_POINT('',#22534);
#6680=VERTEX_POINT('',#22542);
#6681=VERTEX_POINT('',#22549);
#6682=VERTEX_POINT('',#22550);
#6683=VERTEX_POINT('',#22552);
#6684=VERTEX_POINT('',#22554);
#6685=VERTEX_POINT('',#22558);
#6686=VERTEX_POINT('',#22560);
#6687=VERTEX_POINT('',#22564);
#6688=VERTEX_POINT('',#22566);
#6689=VERTEX_POINT('',#22576);
#6690=VERTEX_POINT('',#22577);
#6691=VERTEX_POINT('',#22579);
#6692=VERTEX_POINT('',#22581);
#6693=VERTEX_POINT('',#22585);
#6694=VERTEX_POINT('',#22587);
#6695=VERTEX_POINT('',#22591);
#6696=VERTEX_POINT('',#22593);
#6697=VERTEX_POINT('',#22603);
#6698=VERTEX_POINT('',#22604);
#6699=VERTEX_POINT('',#22606);
#6700=VERTEX_POINT('',#22608);
#6701=VERTEX_POINT('',#22612);
#6702=VERTEX_POINT('',#22614);
#6703=VERTEX_POINT('',#22618);
#6704=VERTEX_POINT('',#22620);
#6705=VERTEX_POINT('',#22630);
#6706=VERTEX_POINT('',#22632);
#6707=VERTEX_POINT('',#22637);
#6708=VERTEX_POINT('',#22639);
#6709=VERTEX_POINT('',#22643);
#6710=VERTEX_POINT('',#22645);
#6711=VERTEX_POINT('',#22649);
#6712=VERTEX_POINT('',#22651);
#6713=VERTEX_POINT('',#22655);
#6714=VERTEX_POINT('',#22657);
#6715=VERTEX_POINT('',#22660);
#6716=VERTEX_POINT('',#22662);
#6717=VERTEX_POINT('',#22667);
#6718=VERTEX_POINT('',#22671);
#6719=VERTEX_POINT('',#22678);
#6720=VERTEX_POINT('',#22680);
#6721=VERTEX_POINT('',#22684);
#6722=VERTEX_POINT('',#22686);
#6723=VERTEX_POINT('',#22693);
#6724=VERTEX_POINT('',#22695);
#6725=VERTEX_POINT('',#22699);
#6726=VERTEX_POINT('',#22701);
#6727=VERTEX_POINT('',#22708);
#6728=VERTEX_POINT('',#22710);
#6729=VERTEX_POINT('',#22714);
#6730=VERTEX_POINT('',#22716);
#6731=VERTEX_POINT('',#22723);
#6732=VERTEX_POINT('',#22725);
#6733=VERTEX_POINT('',#22729);
#6734=VERTEX_POINT('',#22731);
#6735=VERTEX_POINT('',#22738);
#6736=VERTEX_POINT('',#22740);
#6737=VERTEX_POINT('',#22745);
#6738=VERTEX_POINT('',#22747);
#6739=VERTEX_POINT('',#22751);
#6740=VERTEX_POINT('',#22753);
#6741=VERTEX_POINT('',#22757);
#6742=VERTEX_POINT('',#22759);
#6743=VERTEX_POINT('',#22763);
#6744=VERTEX_POINT('',#22765);
#6745=VERTEX_POINT('',#22768);
#6746=VERTEX_POINT('',#22770);
#6747=VERTEX_POINT('',#22775);
#6748=VERTEX_POINT('',#22779);
#6749=VERTEX_POINT('',#22786);
#6750=VERTEX_POINT('',#22788);
#6751=VERTEX_POINT('',#22792);
#6752=VERTEX_POINT('',#22794);
#6753=VERTEX_POINT('',#22801);
#6754=VERTEX_POINT('',#22803);
#6755=VERTEX_POINT('',#22807);
#6756=VERTEX_POINT('',#22809);
#6757=VERTEX_POINT('',#22816);
#6758=VERTEX_POINT('',#22818);
#6759=VERTEX_POINT('',#22822);
#6760=VERTEX_POINT('',#22824);
#6761=VERTEX_POINT('',#22831);
#6762=VERTEX_POINT('',#22834);
#6763=VERTEX_POINT('',#22838);
#6764=VERTEX_POINT('',#22842);
#6765=VERTEX_POINT('',#22846);
#6766=VERTEX_POINT('',#22849);
#6767=VERTEX_POINT('',#22853);
#6768=VERTEX_POINT('',#22857);
#6769=VERTEX_POINT('',#22862);
#6770=VERTEX_POINT('',#22863);
#6771=VERTEX_POINT('',#22865);
#6772=VERTEX_POINT('',#22867);
#6773=VERTEX_POINT('',#22871);
#6774=VERTEX_POINT('',#22873);
#6775=VERTEX_POINT('',#22877);
#6776=VERTEX_POINT('',#22879);
#6777=VERTEX_POINT('',#22883);
#6778=VERTEX_POINT('',#22885);
#6779=VERTEX_POINT('',#22889);
#6780=VERTEX_POINT('',#22891);
#6781=VERTEX_POINT('',#22973);
#6782=VERTEX_POINT('',#22975);
#6783=VERTEX_POINT('',#22979);
#6784=VERTEX_POINT('',#22981);
#6785=VERTEX_POINT('',#22985);
#6786=VERTEX_POINT('',#22987);
#6787=VERTEX_POINT('',#22991);
#6788=VERTEX_POINT('',#22992);
#6789=VERTEX_POINT('',#22994);
#6790=VERTEX_POINT('',#22996);
#6791=VERTEX_POINT('',#23000);
#6792=VERTEX_POINT('',#23002);
#6793=VERTEX_POINT('',#23006);
#6794=VERTEX_POINT('',#23008);
#6795=VERTEX_POINT('',#23018);
#6796=VERTEX_POINT('',#23020);
#6797=VERTEX_POINT('',#23024);
#6798=VERTEX_POINT('',#23026);
#6799=VERTEX_POINT('',#23030);
#6800=VERTEX_POINT('',#23032);
#6801=VERTEX_POINT('',#23036);
#6802=VERTEX_POINT('',#23037);
#6803=VERTEX_POINT('',#23039);
#6804=VERTEX_POINT('',#23041);
#6805=VERTEX_POINT('',#23045);
#6806=VERTEX_POINT('',#23047);
#6807=VERTEX_POINT('',#23051);
#6808=VERTEX_POINT('',#23053);
#6809=VERTEX_POINT('',#23063);
#6810=VERTEX_POINT('',#23065);
#6811=VERTEX_POINT('',#23069);
#6812=VERTEX_POINT('',#23071);
#6813=VERTEX_POINT('',#23075);
#6814=VERTEX_POINT('',#23077);
#6815=VERTEX_POINT('',#23081);
#6816=VERTEX_POINT('',#23082);
#6817=VERTEX_POINT('',#23084);
#6818=VERTEX_POINT('',#23086);
#6819=VERTEX_POINT('',#23090);
#6820=VERTEX_POINT('',#23092);
#6821=VERTEX_POINT('',#23096);
#6822=VERTEX_POINT('',#23098);
#6823=VERTEX_POINT('',#23108);
#6824=VERTEX_POINT('',#23110);
#6825=VERTEX_POINT('',#23114);
#6826=VERTEX_POINT('',#23115);
#6827=VERTEX_POINT('',#23117);
#6828=VERTEX_POINT('',#23119);
#6829=VERTEX_POINT('',#23123);
#6830=VERTEX_POINT('',#23125);
#6831=VERTEX_POINT('',#23129);
#6832=VERTEX_POINT('',#23131);
#6833=VERTEX_POINT('',#23141);
#6834=VERTEX_POINT('',#23143);
#6835=VERTEX_POINT('',#23148);
#6836=VERTEX_POINT('',#23150);
#6837=VERTEX_POINT('',#23153);
#6838=VERTEX_POINT('',#23158);
#6839=VERTEX_POINT('',#23164);
#6840=VERTEX_POINT('',#23166);
#6841=VERTEX_POINT('',#23170);
#6842=VERTEX_POINT('',#23172);
#6843=VERTEX_POINT('',#23179);
#6844=VERTEX_POINT('',#23181);
#6845=VERTEX_POINT('',#23185);
#6846=VERTEX_POINT('',#23187);
#6847=VERTEX_POINT('',#23195);
#6848=VERTEX_POINT('',#23196);
#6849=VERTEX_POINT('',#23198);
#6850=VERTEX_POINT('',#23200);
#6851=VERTEX_POINT('',#23204);
#6852=VERTEX_POINT('',#23206);
#6853=VERTEX_POINT('',#23210);
#6854=VERTEX_POINT('',#23212);
#6855=VERTEX_POINT('',#23220);
#6856=VERTEX_POINT('',#23222);
#6857=VERTEX_POINT('',#23225);
#6858=VERTEX_POINT('',#23229);
#6859=VERTEX_POINT('',#23232);
#6860=VERTEX_POINT('',#23236);
#6861=VERTEX_POINT('',#23239);
#6862=VERTEX_POINT('',#23243);
#6863=VERTEX_POINT('',#23246);
#6864=VERTEX_POINT('',#23250);
#6865=VERTEX_POINT('',#23253);
#6866=VERTEX_POINT('',#23257);
#6867=VERTEX_POINT('',#23263);
#6868=VERTEX_POINT('',#23264);
#6869=VERTEX_POINT('',#23266);
#6870=VERTEX_POINT('',#23268);
#6871=VERTEX_POINT('',#23272);
#6872=VERTEX_POINT('',#23274);
#6873=VERTEX_POINT('',#23278);
#6874=VERTEX_POINT('',#23280);
#6875=VERTEX_POINT('',#23287);
#6876=VERTEX_POINT('',#23289);
#6877=VERTEX_POINT('',#23292);
#6878=VERTEX_POINT('',#23296);
#6879=VERTEX_POINT('',#23304);
#6880=VERTEX_POINT('',#23305);
#6881=VERTEX_POINT('',#23307);
#6882=VERTEX_POINT('',#23309);
#6883=VERTEX_POINT('',#23313);
#6884=VERTEX_POINT('',#23315);
#6885=VERTEX_POINT('',#23319);
#6886=VERTEX_POINT('',#23321);
#6887=VERTEX_POINT('',#23325);
#6888=VERTEX_POINT('',#23327);
#6889=VERTEX_POINT('',#23331);
#6890=VERTEX_POINT('',#23333);
#6891=VERTEX_POINT('',#23342);
#6892=VERTEX_POINT('',#23345);
#6893=VERTEX_POINT('',#23348);
#6894=VERTEX_POINT('',#23352);
#6895=VERTEX_POINT('',#23356);
#6896=VERTEX_POINT('',#23360);
#6897=VERTEX_POINT('',#23363);
#6898=VERTEX_POINT('',#23381);
#6899=VERTEX_POINT('',#23383);
#6900=VERTEX_POINT('',#23387);
#6901=VERTEX_POINT('',#23388);
#6902=VERTEX_POINT('',#23390);
#6903=VERTEX_POINT('',#23392);
#6904=VERTEX_POINT('',#23396);
#6905=VERTEX_POINT('',#23398);
#6906=VERTEX_POINT('',#23401);
#6907=VERTEX_POINT('',#23404);
#6908=VERTEX_POINT('',#23408);
#6909=VERTEX_POINT('',#23412);
#6910=VERTEX_POINT('',#23422);
#6911=VERTEX_POINT('',#23424);
#6912=VERTEX_POINT('',#23431);
#6913=VERTEX_POINT('',#23433);
#6914=VERTEX_POINT('',#23437);
#6915=VERTEX_POINT('',#23439);
#6916=VERTEX_POINT('',#23446);
#6917=VERTEX_POINT('',#23448);
#6918=VERTEX_POINT('',#23452);
#6919=VERTEX_POINT('',#23454);
#6920=VERTEX_POINT('',#23461);
#6921=VERTEX_POINT('',#23463);
#6922=VERTEX_POINT('',#23467);
#6923=VERTEX_POINT('',#23469);
#6924=VERTEX_POINT('',#23476);
#6925=VERTEX_POINT('',#23478);
#6926=EDGE_CURVE('',#5957,#5957,#5199,.T.);
#6927=EDGE_CURVE('',#5957,#5958,#3849,.T.);
#6928=EDGE_CURVE('',#5958,#5958,#5200,.T.);
#6929=EDGE_CURVE('',#5959,#5959,#5201,.T.);
#6930=EDGE_CURVE('',#5959,#5960,#3850,.T.);
#6931=EDGE_CURVE('',#5960,#5960,#5202,.T.);
#6932=EDGE_CURVE('',#5961,#5961,#5203,.T.);
#6933=EDGE_CURVE('',#5961,#5962,#3851,.T.);
#6934=EDGE_CURVE('',#5962,#5962,#5204,.T.);
#6935=EDGE_CURVE('',#5963,#5963,#5205,.T.);
#6936=EDGE_CURVE('',#5963,#5964,#3852,.T.);
#6937=EDGE_CURVE('',#5964,#5964,#5206,.T.);
#6938=EDGE_CURVE('',#5965,#5965,#5207,.T.);
#6939=EDGE_CURVE('',#5965,#5966,#3853,.T.);
#6940=EDGE_CURVE('',#5966,#5966,#5208,.T.);
#6941=EDGE_CURVE('',#5967,#5967,#5209,.T.);
#6942=EDGE_CURVE('',#5967,#5968,#3854,.T.);
#6943=EDGE_CURVE('',#5968,#5968,#5210,.T.);
#6944=EDGE_CURVE('',#5969,#5969,#5211,.T.);
#6945=EDGE_CURVE('',#5969,#5970,#3855,.T.);
#6946=EDGE_CURVE('',#5970,#5970,#5212,.T.);
#6947=EDGE_CURVE('',#5971,#5971,#5213,.T.);
#6948=EDGE_CURVE('',#5971,#5972,#3856,.T.);
#6949=EDGE_CURVE('',#5972,#5972,#5214,.T.);
#6950=EDGE_CURVE('',#5973,#5973,#5215,.T.);
#6951=EDGE_CURVE('',#5973,#5974,#3857,.T.);
#6952=EDGE_CURVE('',#5974,#5974,#5216,.T.);
#6953=EDGE_CURVE('',#5975,#5975,#5217,.T.);
#6954=EDGE_CURVE('',#5975,#5976,#3858,.T.);
#6955=EDGE_CURVE('',#5976,#5976,#5218,.T.);
#6956=EDGE_CURVE('',#5977,#5977,#5219,.T.);
#6957=EDGE_CURVE('',#5977,#5978,#3859,.T.);
#6958=EDGE_CURVE('',#5978,#5978,#5220,.T.);
#6959=EDGE_CURVE('',#5979,#5979,#5221,.T.);
#6960=EDGE_CURVE('',#5979,#5980,#3860,.T.);
#6961=EDGE_CURVE('',#5980,#5980,#5222,.T.);
#6962=EDGE_CURVE('',#5981,#5982,#3861,.T.);
#6963=EDGE_CURVE('',#5982,#5983,#3862,.T.);
#6964=EDGE_CURVE('',#5984,#5983,#3863,.T.);
#6965=EDGE_CURVE('',#5981,#5984,#3864,.T.);
#6966=EDGE_CURVE('',#5985,#5981,#3865,.T.);
#6967=EDGE_CURVE('',#5986,#5984,#3866,.T.);
#6968=EDGE_CURVE('',#5985,#5986,#3867,.T.);
#6969=EDGE_CURVE('',#5987,#5985,#3868,.T.);
#6970=EDGE_CURVE('',#5988,#5986,#3869,.T.);
#6971=EDGE_CURVE('',#5987,#5988,#3870,.T.);
#6972=EDGE_CURVE('',#5982,#5987,#3871,.T.);
#6973=EDGE_CURVE('',#5983,#5988,#3872,.T.);
#6974=EDGE_CURVE('',#5989,#5990,#3873,.T.);
#6975=EDGE_CURVE('',#5990,#5991,#3874,.T.);
#6976=EDGE_CURVE('',#5992,#5991,#3875,.T.);
#6977=EDGE_CURVE('',#5989,#5992,#3876,.T.);
#6978=EDGE_CURVE('',#5993,#5989,#3877,.T.);
#6979=EDGE_CURVE('',#5994,#5992,#3878,.T.);
#6980=EDGE_CURVE('',#5993,#5994,#3879,.T.);
#6981=EDGE_CURVE('',#5995,#5993,#3880,.T.);
#6982=EDGE_CURVE('',#5996,#5994,#3881,.T.);
#6983=EDGE_CURVE('',#5995,#5996,#3882,.T.);
#6984=EDGE_CURVE('',#5990,#5995,#3883,.T.);
#6985=EDGE_CURVE('',#5991,#5996,#3884,.T.);
#6986=EDGE_CURVE('',#5997,#5998,#3885,.T.);
#6987=EDGE_CURVE('',#5998,#5999,#3886,.T.);
#6988=EDGE_CURVE('',#6000,#5999,#3887,.T.);
#6989=EDGE_CURVE('',#5997,#6000,#3888,.T.);
#6990=EDGE_CURVE('',#6001,#5997,#3889,.T.);
#6991=EDGE_CURVE('',#6002,#6000,#3890,.T.);
#6992=EDGE_CURVE('',#6001,#6002,#3891,.T.);
#6993=EDGE_CURVE('',#6003,#6001,#3892,.T.);
#6994=EDGE_CURVE('',#6004,#6002,#3893,.T.);
#6995=EDGE_CURVE('',#6003,#6004,#3894,.T.);
#6996=EDGE_CURVE('',#5998,#6003,#3895,.T.);
#6997=EDGE_CURVE('',#5999,#6004,#3896,.T.);
#6998=EDGE_CURVE('',#6005,#6005,#5223,.T.);
#6999=EDGE_CURVE('',#6005,#6006,#3897,.T.);
#7000=EDGE_CURVE('',#6006,#6006,#5224,.T.);
#7001=EDGE_CURVE('',#6007,#6007,#5225,.T.);
#7002=EDGE_CURVE('',#6007,#6008,#3898,.T.);
#7003=EDGE_CURVE('',#6008,#6008,#5226,.T.);
#7004=EDGE_CURVE('',#6009,#6009,#5227,.T.);
#7005=EDGE_CURVE('',#6009,#6010,#3899,.T.);
#7006=EDGE_CURVE('',#6010,#6010,#5228,.T.);
#7007=EDGE_CURVE('',#6011,#6011,#5229,.T.);
#7008=EDGE_CURVE('',#6011,#6012,#3900,.T.);
#7009=EDGE_CURVE('',#6012,#6012,#5230,.T.);
#7010=EDGE_CURVE('',#6013,#6013,#5231,.T.);
#7011=EDGE_CURVE('',#6013,#6014,#3901,.T.);
#7012=EDGE_CURVE('',#6014,#6014,#5232,.T.);
#7013=EDGE_CURVE('',#6015,#6015,#5233,.T.);
#7014=EDGE_CURVE('',#6015,#6016,#3902,.T.);
#7015=EDGE_CURVE('',#6016,#6016,#5234,.T.);
#7016=EDGE_CURVE('',#6017,#6017,#5235,.T.);
#7017=EDGE_CURVE('',#6017,#6018,#3903,.T.);
#7018=EDGE_CURVE('',#6018,#6018,#5236,.T.);
#7019=EDGE_CURVE('',#6019,#6019,#5237,.T.);
#7020=EDGE_CURVE('',#6019,#6020,#3904,.T.);
#7021=EDGE_CURVE('',#6020,#6020,#5238,.T.);
#7022=EDGE_CURVE('',#6021,#6022,#3905,.T.);
#7023=EDGE_CURVE('',#6023,#6021,#3906,.T.);
#7024=EDGE_CURVE('',#6024,#6023,#3907,.T.);
#7025=EDGE_CURVE('',#6025,#6024,#3908,.T.);
#7026=EDGE_CURVE('',#6025,#6026,#3909,.T.);
#7027=EDGE_CURVE('',#6027,#6026,#3910,.T.);
#7028=EDGE_CURVE('',#6028,#6027,#3911,.T.);
#7029=EDGE_CURVE('',#6022,#6028,#3912,.T.);
#7030=EDGE_CURVE('',#6028,#6029,#3913,.T.);
#7031=EDGE_CURVE('',#6030,#6027,#3914,.T.);
#7032=EDGE_CURVE('',#6029,#6030,#3915,.T.);
#7033=EDGE_CURVE('',#6031,#6025,#3916,.T.);
#7034=EDGE_CURVE('',#6031,#6032,#3917,.T.);
#7035=EDGE_CURVE('',#6026,#6032,#3918,.T.);
#7036=EDGE_CURVE('',#6032,#6030,#3919,.T.);
#7037=EDGE_CURVE('',#6024,#6033,#3920,.T.);
#7038=EDGE_CURVE('',#6034,#6033,#3921,.T.);
#7039=EDGE_CURVE('',#6022,#6034,#3922,.T.);
#7040=EDGE_CURVE('',#6029,#6031,#3923,.T.);
#7041=EDGE_CURVE('',#6023,#6035,#3924,.T.);
#7042=EDGE_CURVE('',#6033,#6035,#3925,.T.);
#7043=EDGE_CURVE('',#6021,#6036,#3926,.T.);
#7044=EDGE_CURVE('',#6035,#6036,#3927,.T.);
#7045=EDGE_CURVE('',#6036,#6034,#3928,.T.);
#7046=EDGE_CURVE('',#6037,#6037,#5239,.T.);
#7047=EDGE_CURVE('',#6037,#6038,#3929,.T.);
#7048=EDGE_CURVE('',#6038,#6038,#5240,.T.);
#7049=EDGE_CURVE('',#6039,#6039,#5241,.T.);
#7050=EDGE_CURVE('',#6039,#6040,#3930,.T.);
#7051=EDGE_CURVE('',#6040,#6040,#5242,.T.);
#7052=EDGE_CURVE('',#6041,#6041,#5243,.T.);
#7053=EDGE_CURVE('',#6041,#6042,#3931,.T.);
#7054=EDGE_CURVE('',#6042,#6042,#5244,.T.);
#7055=EDGE_CURVE('',#6043,#6043,#5245,.T.);
#7056=EDGE_CURVE('',#6043,#6044,#3932,.T.);
#7057=EDGE_CURVE('',#6044,#6044,#5246,.T.);
#7058=EDGE_CURVE('',#6045,#6045,#5247,.T.);
#7059=EDGE_CURVE('',#6045,#6046,#3933,.T.);
#7060=EDGE_CURVE('',#6046,#6046,#5248,.T.);
#7061=EDGE_CURVE('',#6047,#6047,#5249,.T.);
#7062=EDGE_CURVE('',#6047,#6048,#3934,.T.);
#7063=EDGE_CURVE('',#6048,#6048,#5250,.T.);
#7064=EDGE_CURVE('',#6049,#6049,#5251,.T.);
#7065=EDGE_CURVE('',#6049,#6050,#3935,.T.);
#7066=EDGE_CURVE('',#6050,#6050,#5252,.T.);
#7067=EDGE_CURVE('',#6051,#6051,#5253,.T.);
#7068=EDGE_CURVE('',#6051,#6052,#3936,.T.);
#7069=EDGE_CURVE('',#6052,#6052,#5254,.T.);
#7070=EDGE_CURVE('',#6053,#6054,#3937,.T.);
#7071=EDGE_CURVE('',#6055,#6053,#3938,.T.);
#7072=EDGE_CURVE('',#6056,#6055,#3939,.T.);
#7073=EDGE_CURVE('',#6057,#6056,#3940,.T.);
#7074=EDGE_CURVE('',#6057,#6058,#3941,.T.);
#7075=EDGE_CURVE('',#6059,#6058,#3942,.T.);
#7076=EDGE_CURVE('',#6060,#6059,#3943,.T.);
#7077=EDGE_CURVE('',#6054,#6060,#3944,.T.);
#7078=EDGE_CURVE('',#6060,#6061,#3945,.T.);
#7079=EDGE_CURVE('',#6062,#6059,#3946,.T.);
#7080=EDGE_CURVE('',#6061,#6062,#3947,.T.);
#7081=EDGE_CURVE('',#6063,#6057,#3948,.T.);
#7082=EDGE_CURVE('',#6063,#6064,#3949,.T.);
#7083=EDGE_CURVE('',#6058,#6064,#3950,.T.);
#7084=EDGE_CURVE('',#6064,#6062,#3951,.T.);
#7085=EDGE_CURVE('',#6056,#6065,#3952,.T.);
#7086=EDGE_CURVE('',#6066,#6065,#3953,.T.);
#7087=EDGE_CURVE('',#6054,#6066,#3954,.T.);
#7088=EDGE_CURVE('',#6061,#6063,#3955,.T.);
#7089=EDGE_CURVE('',#6055,#6067,#3956,.T.);
#7090=EDGE_CURVE('',#6065,#6067,#3957,.T.);
#7091=EDGE_CURVE('',#6053,#6068,#3958,.T.);
#7092=EDGE_CURVE('',#6067,#6068,#3959,.T.);
#7093=EDGE_CURVE('',#6068,#6066,#3960,.T.);
#7094=EDGE_CURVE('',#6069,#6069,#5255,.T.);
#7095=EDGE_CURVE('',#6069,#6070,#3961,.T.);
#7096=EDGE_CURVE('',#6070,#6070,#5256,.T.);
#7097=EDGE_CURVE('',#6071,#6071,#5257,.T.);
#7098=EDGE_CURVE('',#6071,#6072,#3962,.T.);
#7099=EDGE_CURVE('',#6072,#6072,#5258,.T.);
#7100=EDGE_CURVE('',#6073,#6073,#5259,.T.);
#7101=EDGE_CURVE('',#6073,#6074,#3963,.T.);
#7102=EDGE_CURVE('',#6074,#6074,#5260,.T.);
#7103=EDGE_CURVE('',#6075,#6075,#5261,.T.);
#7104=EDGE_CURVE('',#6075,#6076,#3964,.T.);
#7105=EDGE_CURVE('',#6076,#6076,#5262,.T.);
#7106=EDGE_CURVE('',#6077,#6077,#5263,.T.);
#7107=EDGE_CURVE('',#6078,#6078,#5264,.T.);
#7108=EDGE_CURVE('',#6079,#6079,#5265,.T.);
#7109=EDGE_CURVE('',#6080,#6080,#5266,.T.);
#7110=EDGE_CURVE('',#6077,#6079,#3965,.T.);
#7111=EDGE_CURVE('',#6080,#6081,#3966,.T.);
#7112=EDGE_CURVE('',#6081,#6081,#5267,.T.);
#7113=EDGE_CURVE('',#6082,#6082,#5268,.T.);
#7114=EDGE_CURVE('',#6082,#6078,#3967,.T.);
#7115=EDGE_CURVE('',#6083,#6083,#5269,.T.);
#7116=EDGE_CURVE('',#6083,#6084,#3968,.T.);
#7117=EDGE_CURVE('',#6084,#6084,#5270,.T.);
#7118=EDGE_CURVE('',#6085,#6085,#5271,.T.);
#7119=EDGE_CURVE('',#6085,#6086,#3969,.T.);
#7120=EDGE_CURVE('',#6086,#6086,#5272,.T.);
#7121=EDGE_CURVE('',#6087,#6087,#5273,.T.);
#7122=EDGE_CURVE('',#6087,#6088,#3970,.T.);
#7123=EDGE_CURVE('',#6088,#6088,#5274,.T.);
#7124=EDGE_CURVE('',#6089,#6089,#5275,.T.);
#7125=EDGE_CURVE('',#6089,#6090,#3971,.T.);
#7126=EDGE_CURVE('',#6090,#6090,#5276,.T.);
#7127=EDGE_CURVE('',#6091,#6091,#5277,.T.);
#7128=EDGE_CURVE('',#6091,#6092,#3972,.T.);
#7129=EDGE_CURVE('',#6092,#6092,#5278,.T.);
#7130=EDGE_CURVE('',#6093,#6093,#5279,.T.);
#7131=EDGE_CURVE('',#6093,#6094,#3973,.T.);
#7132=EDGE_CURVE('',#6094,#6094,#5280,.T.);
#7133=EDGE_CURVE('',#6095,#6095,#5281,.T.);
#7134=EDGE_CURVE('',#6095,#6096,#3974,.T.);
#7135=EDGE_CURVE('',#6096,#6096,#5282,.T.);
#7136=EDGE_CURVE('',#6097,#6097,#5283,.T.);
#7137=EDGE_CURVE('',#6097,#6098,#3975,.T.);
#7138=EDGE_CURVE('',#6098,#6098,#5284,.T.);
#7139=EDGE_CURVE('',#6099,#6099,#5285,.T.);
#7140=EDGE_CURVE('',#6099,#6100,#3976,.T.);
#7141=EDGE_CURVE('',#6100,#6100,#5286,.T.);
#7142=EDGE_CURVE('',#6101,#6101,#5287,.T.);
#7143=EDGE_CURVE('',#6101,#6102,#3977,.T.);
#7144=EDGE_CURVE('',#6102,#6102,#5288,.T.);
#7145=EDGE_CURVE('',#6103,#6103,#5289,.T.);
#7146=EDGE_CURVE('',#6104,#6104,#5290,.T.);
#7147=EDGE_CURVE('',#6105,#6105,#5291,.T.);
#7148=EDGE_CURVE('',#6106,#6106,#5292,.T.);
#7149=EDGE_CURVE('',#6103,#6105,#3978,.T.);
#7150=EDGE_CURVE('',#6106,#6107,#3979,.T.);
#7151=EDGE_CURVE('',#6107,#6107,#5293,.T.);
#7152=EDGE_CURVE('',#6108,#6108,#5294,.T.);
#7153=EDGE_CURVE('',#6108,#6104,#3980,.T.);
#7154=EDGE_CURVE('',#6109,#6109,#5295,.T.);
#7155=EDGE_CURVE('',#6109,#6110,#3981,.T.);
#7156=EDGE_CURVE('',#6110,#6110,#5296,.T.);
#7157=EDGE_CURVE('',#6111,#6111,#5297,.T.);
#7158=EDGE_CURVE('',#6111,#6112,#3982,.T.);
#7159=EDGE_CURVE('',#6112,#6112,#5298,.T.);
#7160=EDGE_CURVE('',#6113,#6113,#5299,.T.);
#7161=EDGE_CURVE('',#6113,#6114,#3983,.T.);
#7162=EDGE_CURVE('',#6114,#6114,#5300,.T.);
#7163=EDGE_CURVE('',#6115,#6115,#5301,.T.);
#7164=EDGE_CURVE('',#6115,#6116,#3984,.T.);
#7165=EDGE_CURVE('',#6116,#6116,#5302,.T.);
#7166=EDGE_CURVE('',#6117,#6117,#5303,.T.);
#7167=EDGE_CURVE('',#6117,#6118,#3985,.T.);
#7168=EDGE_CURVE('',#6118,#6118,#5304,.T.);
#7169=EDGE_CURVE('',#6119,#6119,#5305,.T.);
#7170=EDGE_CURVE('',#6119,#6120,#3986,.T.);
#7171=EDGE_CURVE('',#6120,#6120,#5306,.T.);
#7172=EDGE_CURVE('',#6121,#6122,#5307,.T.);
#7173=EDGE_CURVE('',#6123,#6121,#3987,.T.);
#7174=EDGE_CURVE('',#6124,#6123,#5308,.T.);
#7175=EDGE_CURVE('',#6122,#6124,#3988,.T.);
#7176=EDGE_CURVE('',#6125,#6125,#5309,.T.);
#7177=EDGE_CURVE('',#6125,#6126,#3989,.T.);
#7178=EDGE_CURVE('',#6126,#6126,#5310,.T.);
#7179=EDGE_CURVE('',#6121,#6127,#3990,.T.);
#7180=EDGE_CURVE('',#6127,#6128,#3991,.T.);
#7181=EDGE_CURVE('',#6128,#6123,#3992,.T.);
#7182=EDGE_CURVE('',#6129,#6129,#5311,.T.);
#7183=EDGE_CURVE('',#6130,#6128,#3993,.T.);
#7184=EDGE_CURVE('',#6130,#6131,#3994,.T.);
#7185=EDGE_CURVE('',#6131,#6132,#3995,.T.);
#7186=EDGE_CURVE('',#6124,#6132,#3996,.T.);
#7187=EDGE_CURVE('',#6133,#6133,#5312,.T.);
#7188=EDGE_CURVE('',#6134,#6134,#5313,.T.);
#7189=EDGE_CURVE('',#6135,#6135,#5314,.T.);
#7190=EDGE_CURVE('',#6136,#6136,#5315,.T.);
#7191=EDGE_CURVE('',#6136,#6137,#3997,.T.);
#7192=EDGE_CURVE('',#6137,#6137,#5316,.T.);
#7193=EDGE_CURVE('',#6138,#6138,#5317,.T.);
#7194=EDGE_CURVE('',#6139,#6139,#5318,.T.);
#7195=EDGE_CURVE('',#6139,#6138,#3998,.T.);
#7196=EDGE_CURVE('',#6140,#6140,#5319,.T.);
#7197=EDGE_CURVE('',#6140,#6129,#3999,.T.);
#7198=EDGE_CURVE('',#6141,#6141,#5320,.T.);
#7199=EDGE_CURVE('',#6142,#6142,#5321,.T.);
#7200=EDGE_CURVE('',#6142,#6141,#4000,.T.);
#7201=EDGE_CURVE('',#6143,#6143,#5322,.T.);
#7202=EDGE_CURVE('',#6143,#6135,#4001,.T.);
#7203=EDGE_CURVE('',#6144,#6144,#5323,.T.);
#7204=EDGE_CURVE('',#6144,#6134,#4002,.T.);
#7205=EDGE_CURVE('',#6145,#6145,#5324,.T.);
#7206=EDGE_CURVE('',#6145,#6133,#4003,.T.);
#7207=EDGE_CURVE('',#6131,#6146,#4004,.T.);
#7208=EDGE_CURVE('',#6146,#6147,#4005,.T.);
#7209=EDGE_CURVE('',#6132,#6147,#4006,.T.);
#7210=EDGE_CURVE('',#6148,#6130,#4007,.T.);
#7211=EDGE_CURVE('',#6148,#6127,#4008,.T.);
#7212=EDGE_CURVE('',#6147,#6122,#4009,.T.);
#7213=EDGE_CURVE('',#6146,#6148,#4010,.T.);
#7214=EDGE_CURVE('',#6149,#6149,#5325,.T.);
#7215=EDGE_CURVE('',#6149,#6150,#4011,.T.);
#7216=EDGE_CURVE('',#6150,#6150,#5326,.T.);
#7217=EDGE_CURVE('',#6151,#6151,#5327,.T.);
#7218=EDGE_CURVE('',#6151,#6152,#4012,.T.);
#7219=EDGE_CURVE('',#6152,#6152,#5328,.T.);
#7220=EDGE_CURVE('',#6153,#6154,#4013,.T.);
#7221=EDGE_CURVE('',#6155,#6153,#5329,.T.);
#7222=EDGE_CURVE('',#6156,#6155,#4014,.T.);
#7223=EDGE_CURVE('',#6154,#6156,#5330,.T.);
#7224=EDGE_CURVE('',#6157,#6158,#4015,.T.);
#7225=EDGE_CURVE('',#6159,#6157,#5331,.T.);
#7226=EDGE_CURVE('',#6160,#6159,#4016,.T.);
#7227=EDGE_CURVE('',#6158,#6160,#5332,.T.);
#7228=EDGE_CURVE('',#6153,#6159,#5333,.T.);
#7229=EDGE_CURVE('',#6157,#6155,#5334,.T.);
#7230=EDGE_CURVE('',#6161,#6161,#5335,.T.);
#7231=EDGE_CURVE('',#6154,#6160,#5336,.T.);
#7232=EDGE_CURVE('',#6158,#6156,#5337,.T.);
#7233=EDGE_CURVE('',#6161,#6162,#4017,.T.);
#7234=EDGE_CURVE('',#6162,#6162,#5338,.T.);
#7235=EDGE_CURVE('',#6163,#6163,#5339,.T.);
#7236=EDGE_CURVE('',#6164,#6164,#5340,.T.);
#7237=EDGE_CURVE('',#6163,#6165,#4018,.T.);
#7238=EDGE_CURVE('',#6165,#6165,#5341,.T.);
#7239=EDGE_CURVE('',#6166,#6166,#5342,.T.);
#7240=EDGE_CURVE('',#6166,#6164,#4019,.T.);
#7241=EDGE_CURVE('',#6167,#6167,#5343,.T.);
#7242=EDGE_CURVE('',#6168,#6168,#5344,.T.);
#7243=EDGE_CURVE('',#6167,#6169,#4020,.T.);
#7244=EDGE_CURVE('',#6169,#6169,#5345,.T.);
#7245=EDGE_CURVE('',#6170,#6170,#5346,.T.);
#7246=EDGE_CURVE('',#6170,#6168,#4021,.T.);
#7247=EDGE_CURVE('',#6171,#6171,#5347,.T.);
#7248=EDGE_CURVE('',#6171,#6172,#4022,.T.);
#7249=EDGE_CURVE('',#6172,#6172,#5348,.T.);
#7250=EDGE_CURVE('',#6173,#6173,#5349,.T.);
#7251=EDGE_CURVE('',#6173,#6174,#4023,.T.);
#7252=EDGE_CURVE('',#6174,#6174,#5350,.T.);
#7253=EDGE_CURVE('',#6175,#6176,#4024,.T.);
#7254=EDGE_CURVE('',#6177,#6175,#5351,.T.);
#7255=EDGE_CURVE('',#6178,#6177,#4025,.T.);
#7256=EDGE_CURVE('',#6176,#6178,#5352,.T.);
#7257=EDGE_CURVE('',#6179,#6180,#4026,.T.);
#7258=EDGE_CURVE('',#6181,#6179,#5353,.T.);
#7259=EDGE_CURVE('',#6182,#6181,#4027,.T.);
#7260=EDGE_CURVE('',#6180,#6182,#5354,.T.);
#7261=EDGE_CURVE('',#6175,#6181,#5355,.T.);
#7262=EDGE_CURVE('',#6179,#6177,#5356,.T.);
#7263=EDGE_CURVE('',#6183,#6183,#5357,.T.);
#7264=EDGE_CURVE('',#6176,#6182,#5358,.T.);
#7265=EDGE_CURVE('',#6180,#6178,#5359,.T.);
#7266=EDGE_CURVE('',#6183,#6184,#4028,.T.);
#7267=EDGE_CURVE('',#6184,#6184,#5360,.T.);
#7268=EDGE_CURVE('',#6185,#6185,#5361,.T.);
#7269=EDGE_CURVE('',#6186,#6186,#5362,.T.);
#7270=EDGE_CURVE('',#6187,#6187,#5363,.T.);
#7271=EDGE_CURVE('',#6187,#6185,#4029,.T.);
#7272=EDGE_CURVE('',#6186,#6188,#4030,.T.);
#7273=EDGE_CURVE('',#6188,#6188,#5364,.T.);
#7274=EDGE_CURVE('',#6189,#6189,#5365,.T.);
#7275=EDGE_CURVE('',#6190,#6190,#5366,.T.);
#7276=EDGE_CURVE('',#6191,#6191,#5367,.T.);
#7277=EDGE_CURVE('',#6191,#6189,#4031,.T.);
#7278=EDGE_CURVE('',#6190,#6192,#4032,.T.);
#7279=EDGE_CURVE('',#6192,#6192,#5368,.T.);
#7280=EDGE_CURVE('',#6193,#6194,#5369,.T.);
#7281=EDGE_CURVE('',#6195,#6193,#4033,.T.);
#7282=EDGE_CURVE('',#6196,#6195,#5370,.T.);
#7283=EDGE_CURVE('',#6194,#6196,#4034,.T.);
#7284=EDGE_CURVE('',#6197,#6197,#5371,.T.);
#7285=EDGE_CURVE('',#6197,#6198,#4035,.T.);
#7286=EDGE_CURVE('',#6198,#6198,#5372,.T.);
#7287=EDGE_CURVE('',#6193,#6199,#4036,.T.);
#7288=EDGE_CURVE('',#6199,#6200,#4037,.T.);
#7289=EDGE_CURVE('',#6200,#6195,#4038,.T.);
#7290=EDGE_CURVE('',#6201,#6201,#5373,.T.);
#7291=EDGE_CURVE('',#6202,#6200,#4039,.T.);
#7292=EDGE_CURVE('',#6202,#6203,#4040,.T.);
#7293=EDGE_CURVE('',#6203,#6204,#4041,.T.);
#7294=EDGE_CURVE('',#6196,#6204,#4042,.T.);
#7295=EDGE_CURVE('',#6205,#6205,#5374,.T.);
#7296=EDGE_CURVE('',#6206,#6206,#5375,.T.);
#7297=EDGE_CURVE('',#6207,#6207,#5376,.T.);
#7298=EDGE_CURVE('',#6208,#6208,#5377,.T.);
#7299=EDGE_CURVE('',#6208,#6209,#4043,.T.);
#7300=EDGE_CURVE('',#6209,#6209,#5378,.T.);
#7301=EDGE_CURVE('',#6210,#6210,#5379,.T.);
#7302=EDGE_CURVE('',#6211,#6211,#5380,.T.);
#7303=EDGE_CURVE('',#6211,#6210,#4044,.T.);
#7304=EDGE_CURVE('',#6212,#6212,#5381,.T.);
#7305=EDGE_CURVE('',#6212,#6201,#4045,.T.);
#7306=EDGE_CURVE('',#6213,#6213,#5382,.T.);
#7307=EDGE_CURVE('',#6214,#6214,#5383,.T.);
#7308=EDGE_CURVE('',#6214,#6213,#4046,.T.);
#7309=EDGE_CURVE('',#6215,#6215,#5384,.T.);
#7310=EDGE_CURVE('',#6215,#6207,#4047,.T.);
#7311=EDGE_CURVE('',#6216,#6216,#5385,.T.);
#7312=EDGE_CURVE('',#6216,#6206,#4048,.T.);
#7313=EDGE_CURVE('',#6217,#6217,#5386,.T.);
#7314=EDGE_CURVE('',#6217,#6205,#4049,.T.);
#7315=EDGE_CURVE('',#6203,#6218,#4050,.T.);
#7316=EDGE_CURVE('',#6218,#6219,#4051,.T.);
#7317=EDGE_CURVE('',#6204,#6219,#4052,.T.);
#7318=EDGE_CURVE('',#6220,#6202,#4053,.T.);
#7319=EDGE_CURVE('',#6220,#6199,#4054,.T.);
#7320=EDGE_CURVE('',#6219,#6194,#4055,.T.);
#7321=EDGE_CURVE('',#6218,#6220,#4056,.T.);
#7322=EDGE_CURVE('',#6221,#6221,#5387,.T.);
#7323=EDGE_CURVE('',#6221,#6222,#4057,.T.);
#7324=EDGE_CURVE('',#6222,#6222,#5388,.T.);
#7325=EDGE_CURVE('',#6223,#6223,#5389,.T.);
#7326=EDGE_CURVE('',#6223,#6224,#4058,.T.);
#7327=EDGE_CURVE('',#6224,#6224,#5390,.T.);
#7328=EDGE_CURVE('',#6225,#6226,#4059,.T.);
#7329=EDGE_CURVE('',#6227,#6225,#5391,.T.);
#7330=EDGE_CURVE('',#6228,#6227,#4060,.T.);
#7331=EDGE_CURVE('',#6226,#6228,#5392,.T.);
#7332=EDGE_CURVE('',#6229,#6230,#4061,.T.);
#7333=EDGE_CURVE('',#6231,#6229,#5393,.T.);
#7334=EDGE_CURVE('',#6232,#6231,#4062,.T.);
#7335=EDGE_CURVE('',#6230,#6232,#5394,.T.);
#7336=EDGE_CURVE('',#6225,#6231,#5395,.T.);
#7337=EDGE_CURVE('',#6229,#6227,#5396,.T.);
#7338=EDGE_CURVE('',#6233,#6233,#5397,.T.);
#7339=EDGE_CURVE('',#6226,#6232,#5398,.T.);
#7340=EDGE_CURVE('',#6230,#6228,#5399,.T.);
#7341=EDGE_CURVE('',#6233,#6234,#4063,.T.);
#7342=EDGE_CURVE('',#6234,#6234,#5400,.T.);
#7343=EDGE_CURVE('',#6235,#6235,#5401,.T.);
#7344=EDGE_CURVE('',#6236,#6236,#5402,.T.);
#7345=EDGE_CURVE('',#6235,#6237,#4064,.T.);
#7346=EDGE_CURVE('',#6237,#6237,#5403,.T.);
#7347=EDGE_CURVE('',#6238,#6238,#5404,.T.);
#7348=EDGE_CURVE('',#6238,#6236,#4065,.T.);
#7349=EDGE_CURVE('',#6239,#6239,#5405,.T.);
#7350=EDGE_CURVE('',#6240,#6240,#5406,.T.);
#7351=EDGE_CURVE('',#6239,#6241,#4066,.T.);
#7352=EDGE_CURVE('',#6241,#6241,#5407,.T.);
#7353=EDGE_CURVE('',#6242,#6242,#5408,.T.);
#7354=EDGE_CURVE('',#6242,#6240,#4067,.T.);
#7355=EDGE_CURVE('',#6243,#6243,#5409,.T.);
#7356=EDGE_CURVE('',#6243,#6244,#4068,.T.);
#7357=EDGE_CURVE('',#6244,#6244,#5410,.T.);
#7358=EDGE_CURVE('',#6245,#6245,#5411,.T.);
#7359=EDGE_CURVE('',#6245,#6246,#4069,.T.);
#7360=EDGE_CURVE('',#6246,#6246,#5412,.T.);
#7361=EDGE_CURVE('',#6247,#6248,#4070,.T.);
#7362=EDGE_CURVE('',#6249,#6247,#5413,.T.);
#7363=EDGE_CURVE('',#6250,#6249,#4071,.T.);
#7364=EDGE_CURVE('',#6248,#6250,#5414,.T.);
#7365=EDGE_CURVE('',#6251,#6252,#4072,.T.);
#7366=EDGE_CURVE('',#6253,#6251,#5415,.T.);
#7367=EDGE_CURVE('',#6254,#6253,#4073,.T.);
#7368=EDGE_CURVE('',#6252,#6254,#5416,.T.);
#7369=EDGE_CURVE('',#6247,#6253,#5417,.T.);
#7370=EDGE_CURVE('',#6251,#6249,#5418,.T.);
#7371=EDGE_CURVE('',#6255,#6255,#5419,.T.);
#7372=EDGE_CURVE('',#6248,#6254,#5420,.T.);
#7373=EDGE_CURVE('',#6252,#6250,#5421,.T.);
#7374=EDGE_CURVE('',#6255,#6256,#4074,.T.);
#7375=EDGE_CURVE('',#6256,#6256,#5422,.T.);
#7376=EDGE_CURVE('',#6257,#6257,#5423,.T.);
#7377=EDGE_CURVE('',#6258,#6258,#5424,.T.);
#7378=EDGE_CURVE('',#6259,#6259,#5425,.T.);
#7379=EDGE_CURVE('',#6259,#6257,#4075,.T.);
#7380=EDGE_CURVE('',#6258,#6260,#4076,.T.);
#7381=EDGE_CURVE('',#6260,#6260,#5426,.T.);
#7382=EDGE_CURVE('',#6261,#6261,#5427,.T.);
#7383=EDGE_CURVE('',#6262,#6262,#5428,.T.);
#7384=EDGE_CURVE('',#6263,#6263,#5429,.T.);
#7385=EDGE_CURVE('',#6263,#6261,#4077,.T.);
#7386=EDGE_CURVE('',#6262,#6264,#4078,.T.);
#7387=EDGE_CURVE('',#6264,#6264,#5430,.T.);
#7388=EDGE_CURVE('',#6265,#6265,#5431,.T.);
#7389=EDGE_CURVE('',#6265,#6266,#4079,.T.);
#7390=EDGE_CURVE('',#6266,#6266,#5432,.T.);
#7391=EDGE_CURVE('',#6267,#6267,#5433,.T.);
#7392=EDGE_CURVE('',#6267,#6268,#4080,.T.);
#7393=EDGE_CURVE('',#6268,#6268,#5434,.T.);
#7394=EDGE_CURVE('',#6269,#6269,#5435,.T.);
#7395=EDGE_CURVE('',#6270,#6270,#5436,.T.);
#7396=EDGE_CURVE('',#6270,#6269,#4081,.T.);
#7397=EDGE_CURVE('',#6271,#6271,#5437,.T.);
#7398=EDGE_CURVE('',#6271,#6270,#4082,.T.);
#7399=EDGE_CURVE('',#6272,#6272,#5438,.T.);
#7400=EDGE_CURVE('',#6272,#6271,#4083,.T.);
#7401=EDGE_CURVE('',#6273,#6273,#5439,.T.);
#7402=EDGE_CURVE('',#6274,#6274,#5440,.F.);
#7403=EDGE_CURVE('',#6274,#6273,#4084,.T.);
#7404=EDGE_CURVE('',#6275,#6275,#5441,.F.);
#7405=EDGE_CURVE('',#6275,#6274,#4085,.T.);
#7406=EDGE_CURVE('',#6276,#6276,#5442,.T.);
#7407=EDGE_CURVE('',#6276,#6275,#4086,.T.);
#7408=EDGE_CURVE('',#6277,#6278,#4087,.T.);
#7409=EDGE_CURVE('',#6278,#6279,#4088,.T.);
#7410=EDGE_CURVE('',#6279,#6280,#4089,.T.);
#7411=EDGE_CURVE('',#6277,#6280,#4090,.T.);
#7412=EDGE_CURVE('',#6278,#6281,#4091,.T.);
#7413=EDGE_CURVE('',#6281,#6282,#4092,.T.);
#7414=EDGE_CURVE('',#6282,#6279,#4093,.T.);
#7415=EDGE_CURVE('',#6281,#6283,#4094,.T.);
#7416=EDGE_CURVE('',#6283,#6284,#4095,.T.);
#7417=EDGE_CURVE('',#6284,#6282,#4096,.T.);
#7418=EDGE_CURVE('',#6283,#6285,#4097,.T.);
#7419=EDGE_CURVE('',#6285,#6286,#4098,.T.);
#7420=EDGE_CURVE('',#6286,#6284,#4099,.T.);
#7421=EDGE_CURVE('',#6285,#6287,#4100,.T.);
#7422=EDGE_CURVE('',#6287,#6288,#4101,.T.);
#7423=EDGE_CURVE('',#6288,#6286,#4102,.T.);
#7424=EDGE_CURVE('',#6287,#6277,#4103,.T.);
#7425=EDGE_CURVE('',#6280,#6288,#4104,.T.);
#7426=EDGE_CURVE('',#6289,#6289,#5443,.T.);
#7427=EDGE_CURVE('',#6289,#6290,#4105,.T.);
#7428=EDGE_CURVE('',#6290,#6290,#5444,.T.);
#7429=EDGE_CURVE('',#6291,#6291,#5445,.T.);
#7430=EDGE_CURVE('',#6291,#6292,#4106,.T.);
#7431=EDGE_CURVE('',#6292,#6292,#5446,.T.);
#7432=EDGE_CURVE('',#6293,#6293,#5447,.T.);
#7433=EDGE_CURVE('',#6293,#6294,#4107,.T.);
#7434=EDGE_CURVE('',#6294,#6294,#5448,.T.);
#7435=EDGE_CURVE('',#6295,#6295,#5449,.T.);
#7436=EDGE_CURVE('',#6295,#6296,#4108,.T.);
#7437=EDGE_CURVE('',#6296,#6296,#5450,.T.);
#7438=EDGE_CURVE('',#6297,#6297,#5451,.T.);
#7439=EDGE_CURVE('',#6297,#6298,#4109,.T.);
#7440=EDGE_CURVE('',#6298,#6298,#5452,.T.);
#7441=EDGE_CURVE('',#6299,#6300,#4110,.T.);
#7442=EDGE_CURVE('',#6301,#6299,#5453,.T.);
#7443=EDGE_CURVE('',#6302,#6301,#4111,.T.);
#7444=EDGE_CURVE('',#6302,#6300,#5454,.T.);
#7445=EDGE_CURVE('',#6303,#6302,#4112,.T.);
#7446=EDGE_CURVE('',#6304,#6303,#5455,.T.);
#7447=EDGE_CURVE('',#6300,#6304,#4113,.T.);
#7448=EDGE_CURVE('',#6305,#6305,#5456,.T.);
#7449=EDGE_CURVE('',#6306,#6306,#5457,.T.);
#7450=EDGE_CURVE('',#6307,#6307,#5458,.T.);
#7451=EDGE_CURVE('',#6308,#6308,#5459,.T.);
#7452=EDGE_CURVE('',#6309,#6309,#5460,.T.);
#7453=EDGE_CURVE('',#6310,#6301,#4114,.T.);
#7454=EDGE_CURVE('',#6310,#6303,#4115,.T.);
#7455=EDGE_CURVE('',#6309,#6311,#4116,.T.);
#7456=EDGE_CURVE('',#6311,#6311,#5461,.T.);
#7457=EDGE_CURVE('',#6308,#6312,#4117,.T.);
#7458=EDGE_CURVE('',#6312,#6312,#5462,.T.);
#7459=EDGE_CURVE('',#6307,#6313,#4118,.T.);
#7460=EDGE_CURVE('',#6313,#6313,#5463,.T.);
#7461=EDGE_CURVE('',#6306,#6314,#4119,.T.);
#7462=EDGE_CURVE('',#6314,#6314,#5464,.T.);
#7463=EDGE_CURVE('',#6305,#6315,#4120,.T.);
#7464=EDGE_CURVE('',#6315,#6315,#5465,.T.);
#7465=EDGE_CURVE('',#6304,#6316,#4121,.T.);
#7466=EDGE_CURVE('',#6316,#6310,#5466,.T.);
#7467=EDGE_CURVE('',#6299,#6316,#4122,.T.);
#7468=EDGE_CURVE('',#6317,#6317,#5467,.T.);
#7469=EDGE_CURVE('',#6317,#6318,#4123,.T.);
#7470=EDGE_CURVE('',#6318,#6318,#5468,.T.);
#7471=EDGE_CURVE('',#6319,#6319,#5469,.T.);
#7472=EDGE_CURVE('',#6319,#6320,#4124,.T.);
#7473=EDGE_CURVE('',#6320,#6320,#5470,.T.);
#7474=EDGE_CURVE('',#6321,#6321,#5471,.T.);
#7475=EDGE_CURVE('',#6321,#6322,#4125,.T.);
#7476=EDGE_CURVE('',#6322,#6322,#5472,.T.);
#7477=EDGE_CURVE('',#6323,#6323,#5473,.T.);
#7478=EDGE_CURVE('',#6323,#6324,#4126,.T.);
#7479=EDGE_CURVE('',#6324,#6324,#5474,.T.);
#7480=EDGE_CURVE('',#6325,#6325,#5475,.T.);
#7481=EDGE_CURVE('',#6325,#6326,#4127,.T.);
#7482=EDGE_CURVE('',#6326,#6326,#5476,.T.);
#7483=EDGE_CURVE('',#6327,#6327,#5477,.T.);
#7484=EDGE_CURVE('',#6327,#6328,#4128,.T.);
#7485=EDGE_CURVE('',#6328,#6328,#5478,.T.);
#7486=EDGE_CURVE('',#6329,#6329,#5479,.T.);
#7487=EDGE_CURVE('',#6330,#6330,#5480,.T.);
#7488=EDGE_CURVE('',#6329,#6331,#4129,.T.);
#7489=EDGE_CURVE('',#6331,#6331,#5481,.T.);
#7490=EDGE_CURVE('',#6332,#6332,#5482,.T.);
#7491=EDGE_CURVE('',#6332,#6330,#4130,.T.);
#7492=EDGE_CURVE('',#6333,#6333,#5483,.T.);
#7493=EDGE_CURVE('',#6334,#6334,#5484,.T.);
#7494=EDGE_CURVE('',#6333,#6335,#4131,.T.);
#7495=EDGE_CURVE('',#6335,#6335,#5485,.T.);
#7496=EDGE_CURVE('',#6336,#6336,#5486,.T.);
#7497=EDGE_CURVE('',#6336,#6334,#4132,.T.);
#7498=EDGE_CURVE('',#6337,#6337,#5487,.T.);
#7499=EDGE_CURVE('',#6338,#6338,#5488,.T.);
#7500=EDGE_CURVE('',#6337,#6339,#4133,.T.);
#7501=EDGE_CURVE('',#6339,#6339,#5489,.T.);
#7502=EDGE_CURVE('',#6340,#6340,#5490,.T.);
#7503=EDGE_CURVE('',#6340,#6338,#4134,.T.);
#7504=EDGE_CURVE('',#6341,#6341,#5491,.T.);
#7505=EDGE_CURVE('',#6342,#6342,#5492,.T.);
#7506=EDGE_CURVE('',#6341,#6343,#4135,.T.);
#7507=EDGE_CURVE('',#6343,#6343,#5493,.T.);
#7508=EDGE_CURVE('',#6344,#6344,#5494,.T.);
#7509=EDGE_CURVE('',#6344,#6342,#4136,.T.);
#7510=EDGE_CURVE('',#6345,#6345,#5495,.T.);
#7511=EDGE_CURVE('',#6345,#6346,#4137,.T.);
#7512=EDGE_CURVE('',#6346,#6346,#5496,.T.);
#7513=EDGE_CURVE('',#6347,#6347,#5497,.T.);
#7514=EDGE_CURVE('',#6347,#6348,#4138,.T.);
#7515=EDGE_CURVE('',#6348,#6348,#5498,.T.);
#7516=EDGE_CURVE('',#6349,#6349,#5499,.T.);
#7517=EDGE_CURVE('',#6349,#6350,#4139,.T.);
#7518=EDGE_CURVE('',#6350,#6350,#5500,.T.);
#7519=EDGE_CURVE('',#6351,#6351,#5501,.T.);
#7520=EDGE_CURVE('',#6351,#6352,#4140,.T.);
#7521=EDGE_CURVE('',#6352,#6352,#5502,.T.);
#7522=EDGE_CURVE('',#6353,#6353,#5503,.T.);
#7523=EDGE_CURVE('',#6353,#6354,#4141,.T.);
#7524=EDGE_CURVE('',#6354,#6354,#5504,.T.);
#7525=EDGE_CURVE('',#6355,#6355,#5505,.T.);
#7526=EDGE_CURVE('',#6355,#6356,#4142,.T.);
#7527=EDGE_CURVE('',#6356,#6356,#5506,.T.);
#7528=EDGE_CURVE('',#6357,#6357,#5507,.T.);
#7529=EDGE_CURVE('',#6358,#6358,#5508,.T.);
#7530=EDGE_CURVE('',#6359,#6359,#5509,.T.);
#7531=EDGE_CURVE('',#6359,#6357,#4143,.T.);
#7532=EDGE_CURVE('',#6358,#6360,#4144,.T.);
#7533=EDGE_CURVE('',#6360,#6360,#5510,.T.);
#7534=EDGE_CURVE('',#6361,#6361,#5511,.T.);
#7535=EDGE_CURVE('',#6362,#6362,#5512,.T.);
#7536=EDGE_CURVE('',#6363,#6363,#5513,.T.);
#7537=EDGE_CURVE('',#6363,#6361,#4145,.T.);
#7538=EDGE_CURVE('',#6362,#6364,#4146,.T.);
#7539=EDGE_CURVE('',#6364,#6364,#5514,.T.);
#7540=EDGE_CURVE('',#6365,#6365,#5515,.T.);
#7541=EDGE_CURVE('',#6366,#6366,#5516,.T.);
#7542=EDGE_CURVE('',#6367,#6367,#5517,.T.);
#7543=EDGE_CURVE('',#6367,#6365,#4147,.T.);
#7544=EDGE_CURVE('',#6366,#6368,#4148,.T.);
#7545=EDGE_CURVE('',#6368,#6368,#5518,.T.);
#7546=EDGE_CURVE('',#6369,#6369,#5519,.T.);
#7547=EDGE_CURVE('',#6370,#6370,#5520,.T.);
#7548=EDGE_CURVE('',#6371,#6371,#5521,.T.);
#7549=EDGE_CURVE('',#6371,#6369,#4149,.T.);
#7550=EDGE_CURVE('',#6370,#6372,#4150,.T.);
#7551=EDGE_CURVE('',#6372,#6372,#5522,.T.);
#7552=EDGE_CURVE('',#6373,#6373,#5523,.T.);
#7553=EDGE_CURVE('',#6373,#6374,#4151,.T.);
#7554=EDGE_CURVE('',#6374,#6374,#5524,.T.);
#7555=EDGE_CURVE('',#6375,#6375,#5525,.T.);
#7556=EDGE_CURVE('',#6375,#6376,#4152,.T.);
#7557=EDGE_CURVE('',#6376,#6376,#5526,.T.);
#7558=EDGE_CURVE('',#6377,#6377,#5527,.T.);
#7559=EDGE_CURVE('',#6377,#6378,#4153,.T.);
#7560=EDGE_CURVE('',#6378,#6378,#5528,.T.);
#7561=EDGE_CURVE('',#6379,#6379,#5529,.T.);
#7562=EDGE_CURVE('',#6379,#6380,#4154,.T.);
#7563=EDGE_CURVE('',#6380,#6380,#5530,.T.);
#7564=EDGE_CURVE('',#6381,#6381,#5531,.T.);
#7565=EDGE_CURVE('',#6381,#6382,#4155,.T.);
#7566=EDGE_CURVE('',#6382,#6382,#5532,.T.);
#7567=EDGE_CURVE('',#6383,#6383,#5533,.T.);
#7568=EDGE_CURVE('',#6383,#6384,#4156,.T.);
#7569=EDGE_CURVE('',#6384,#6384,#5534,.T.);
#7570=EDGE_CURVE('',#6385,#6385,#5535,.T.);
#7571=EDGE_CURVE('',#6386,#6386,#5536,.T.);
#7572=EDGE_CURVE('',#6385,#6387,#4157,.T.);
#7573=EDGE_CURVE('',#6387,#6387,#5537,.T.);
#7574=EDGE_CURVE('',#6388,#6388,#5538,.T.);
#7575=EDGE_CURVE('',#6388,#6386,#4158,.T.);
#7576=EDGE_CURVE('',#6389,#6389,#5539,.T.);
#7577=EDGE_CURVE('',#6390,#6390,#5540,.T.);
#7578=EDGE_CURVE('',#6389,#6391,#4159,.T.);
#7579=EDGE_CURVE('',#6391,#6391,#5541,.T.);
#7580=EDGE_CURVE('',#6392,#6392,#5542,.T.);
#7581=EDGE_CURVE('',#6392,#6390,#4160,.T.);
#7582=EDGE_CURVE('',#6393,#6393,#5543,.T.);
#7583=EDGE_CURVE('',#6394,#6394,#5544,.T.);
#7584=EDGE_CURVE('',#6393,#6395,#4161,.T.);
#7585=EDGE_CURVE('',#6395,#6395,#5545,.T.);
#7586=EDGE_CURVE('',#6396,#6396,#5546,.T.);
#7587=EDGE_CURVE('',#6396,#6394,#4162,.T.);
#7588=EDGE_CURVE('',#6397,#6397,#5547,.T.);
#7589=EDGE_CURVE('',#6398,#6398,#5548,.T.);
#7590=EDGE_CURVE('',#6397,#6399,#4163,.T.);
#7591=EDGE_CURVE('',#6399,#6399,#5549,.T.);
#7592=EDGE_CURVE('',#6400,#6400,#5550,.T.);
#7593=EDGE_CURVE('',#6400,#6398,#4164,.T.);
#7594=EDGE_CURVE('',#6401,#6401,#5551,.T.);
#7595=EDGE_CURVE('',#6401,#6402,#4165,.T.);
#7596=EDGE_CURVE('',#6402,#6402,#5552,.T.);
#7597=EDGE_CURVE('',#6403,#6403,#5553,.T.);
#7598=EDGE_CURVE('',#6403,#6404,#4166,.T.);
#7599=EDGE_CURVE('',#6404,#6404,#5554,.T.);
#7600=EDGE_CURVE('',#6405,#6405,#5555,.T.);
#7601=EDGE_CURVE('',#6405,#6406,#4167,.T.);
#7602=EDGE_CURVE('',#6406,#6406,#5556,.T.);
#7603=EDGE_CURVE('',#6407,#6407,#5557,.T.);
#7604=EDGE_CURVE('',#6407,#6408,#4168,.T.);
#7605=EDGE_CURVE('',#6408,#6408,#5558,.T.);
#7606=EDGE_CURVE('',#6409,#6409,#5559,.T.);
#7607=EDGE_CURVE('',#6409,#6410,#4169,.T.);
#7608=EDGE_CURVE('',#6410,#6410,#5560,.T.);
#7609=EDGE_CURVE('',#6411,#6411,#5561,.T.);
#7610=EDGE_CURVE('',#6411,#6412,#4170,.T.);
#7611=EDGE_CURVE('',#6412,#6412,#5562,.T.);
#7612=EDGE_CURVE('',#6413,#6413,#5563,.T.);
#7613=EDGE_CURVE('',#6414,#6414,#5564,.T.);
#7614=EDGE_CURVE('',#6415,#6415,#5565,.T.);
#7615=EDGE_CURVE('',#6415,#6413,#4171,.T.);
#7616=EDGE_CURVE('',#6414,#6416,#4172,.T.);
#7617=EDGE_CURVE('',#6416,#6416,#5566,.T.);
#7618=EDGE_CURVE('',#6417,#6417,#5567,.T.);
#7619=EDGE_CURVE('',#6418,#6418,#5568,.T.);
#7620=EDGE_CURVE('',#6419,#6419,#5569,.T.);
#7621=EDGE_CURVE('',#6419,#6417,#4173,.T.);
#7622=EDGE_CURVE('',#6418,#6420,#4174,.T.);
#7623=EDGE_CURVE('',#6420,#6420,#5570,.T.);
#7624=EDGE_CURVE('',#6421,#6421,#5571,.T.);
#7625=EDGE_CURVE('',#6422,#6422,#5572,.T.);
#7626=EDGE_CURVE('',#6423,#6423,#5573,.T.);
#7627=EDGE_CURVE('',#6423,#6421,#4175,.T.);
#7628=EDGE_CURVE('',#6422,#6424,#4176,.T.);
#7629=EDGE_CURVE('',#6424,#6424,#5574,.T.);
#7630=EDGE_CURVE('',#6425,#6425,#5575,.T.);
#7631=EDGE_CURVE('',#6426,#6426,#5576,.T.);
#7632=EDGE_CURVE('',#6427,#6427,#5577,.T.);
#7633=EDGE_CURVE('',#6427,#6425,#4177,.T.);
#7634=EDGE_CURVE('',#6426,#6428,#4178,.T.);
#7635=EDGE_CURVE('',#6428,#6428,#5578,.T.);
#7636=EDGE_CURVE('',#6429,#6429,#5579,.T.);
#7637=EDGE_CURVE('',#6429,#6430,#4179,.T.);
#7638=EDGE_CURVE('',#6430,#6430,#5580,.T.);
#7639=EDGE_CURVE('',#6431,#6431,#5581,.T.);
#7640=EDGE_CURVE('',#6431,#6432,#4180,.T.);
#7641=EDGE_CURVE('',#6432,#6432,#5582,.T.);
#7642=EDGE_CURVE('',#6433,#6433,#5583,.T.);
#7643=EDGE_CURVE('',#6433,#6434,#4181,.T.);
#7644=EDGE_CURVE('',#6434,#6434,#5584,.T.);
#7645=EDGE_CURVE('',#6435,#6435,#5585,.T.);
#7646=EDGE_CURVE('',#6435,#6436,#4182,.T.);
#7647=EDGE_CURVE('',#6436,#6436,#5586,.T.);
#7648=EDGE_CURVE('',#6437,#6437,#5587,.T.);
#7649=EDGE_CURVE('',#6437,#6438,#4183,.T.);
#7650=EDGE_CURVE('',#6438,#6438,#5588,.T.);
#7651=EDGE_CURVE('',#6439,#6440,#4184,.T.);
#7652=EDGE_CURVE('',#6439,#6441,#5589,.T.);
#7653=EDGE_CURVE('',#6442,#6441,#4185,.T.);
#7654=EDGE_CURVE('',#6440,#6442,#5590,.T.);
#7655=EDGE_CURVE('',#6443,#6440,#4186,.T.);
#7656=EDGE_CURVE('',#6443,#6444,#4187,.T.);
#7657=EDGE_CURVE('',#6444,#6439,#4188,.T.);
#7658=EDGE_CURVE('',#6442,#6445,#4189,.T.);
#7659=EDGE_CURVE('',#6445,#6443,#5591,.T.);
#7660=EDGE_CURVE('',#6446,#6446,#5592,.T.);
#7661=EDGE_CURVE('',#6447,#6447,#5593,.T.);
#7662=EDGE_CURVE('',#6448,#6448,#5594,.T.);
#7663=EDGE_CURVE('',#6449,#6449,#5595,.T.);
#7664=EDGE_CURVE('',#6450,#6450,#5596,.T.);
#7665=EDGE_CURVE('',#6451,#6451,#5597,.T.);
#7666=EDGE_CURVE('',#6451,#6450,#4190,.T.);
#7667=EDGE_CURVE('',#6452,#6452,#5598,.T.);
#7668=EDGE_CURVE('',#6452,#6449,#4191,.T.);
#7669=EDGE_CURVE('',#6453,#6453,#5599,.T.);
#7670=EDGE_CURVE('',#6453,#6448,#4192,.T.);
#7671=EDGE_CURVE('',#6454,#6454,#5600,.T.);
#7672=EDGE_CURVE('',#6454,#6447,#4193,.T.);
#7673=EDGE_CURVE('',#6455,#6455,#5601,.T.);
#7674=EDGE_CURVE('',#6455,#6446,#4194,.T.);
#7675=EDGE_CURVE('',#6456,#6445,#4195,.T.);
#7676=EDGE_CURVE('',#6456,#6444,#5602,.T.);
#7677=EDGE_CURVE('',#6441,#6456,#4196,.T.);
#7678=EDGE_CURVE('',#6457,#6457,#5603,.T.);
#7679=EDGE_CURVE('',#6457,#6458,#4197,.T.);
#7680=EDGE_CURVE('',#6458,#6458,#5604,.T.);
#7681=EDGE_CURVE('',#6459,#6459,#5605,.T.);
#7682=EDGE_CURVE('',#6459,#6460,#4198,.T.);
#7683=EDGE_CURVE('',#6460,#6460,#5606,.T.);
#7684=EDGE_CURVE('',#6461,#6461,#5607,.T.);
#7685=EDGE_CURVE('',#6461,#6462,#4199,.T.);
#7686=EDGE_CURVE('',#6462,#6462,#5608,.T.);
#7687=EDGE_CURVE('',#6463,#6463,#5609,.T.);
#7688=EDGE_CURVE('',#6463,#6464,#4200,.T.);
#7689=EDGE_CURVE('',#6464,#6464,#5610,.T.);
#7690=EDGE_CURVE('',#6465,#6465,#5611,.T.);
#7691=EDGE_CURVE('',#6465,#6466,#4201,.T.);
#7692=EDGE_CURVE('',#6466,#6466,#5612,.T.);
#7693=EDGE_CURVE('',#6467,#6467,#5613,.T.);
#7694=EDGE_CURVE('',#6467,#6468,#4202,.T.);
#7695=EDGE_CURVE('',#6468,#6468,#5614,.T.);
#7696=EDGE_CURVE('',#6469,#6469,#5615,.T.);
#7697=EDGE_CURVE('',#6470,#6470,#5616,.T.);
#7698=EDGE_CURVE('',#6469,#6471,#4203,.T.);
#7699=EDGE_CURVE('',#6471,#6471,#5617,.T.);
#7700=EDGE_CURVE('',#6472,#6472,#5618,.T.);
#7701=EDGE_CURVE('',#6472,#6470,#4204,.T.);
#7702=EDGE_CURVE('',#6473,#6473,#5619,.T.);
#7703=EDGE_CURVE('',#6474,#6474,#5620,.T.);
#7704=EDGE_CURVE('',#6473,#6475,#4205,.T.);
#7705=EDGE_CURVE('',#6475,#6475,#5621,.T.);
#7706=EDGE_CURVE('',#6476,#6476,#5622,.T.);
#7707=EDGE_CURVE('',#6476,#6474,#4206,.T.);
#7708=EDGE_CURVE('',#6477,#6477,#5623,.T.);
#7709=EDGE_CURVE('',#6478,#6478,#5624,.T.);
#7710=EDGE_CURVE('',#6477,#6479,#4207,.T.);
#7711=EDGE_CURVE('',#6479,#6479,#5625,.T.);
#7712=EDGE_CURVE('',#6480,#6480,#5626,.T.);
#7713=EDGE_CURVE('',#6480,#6478,#4208,.T.);
#7714=EDGE_CURVE('',#6481,#6481,#5627,.T.);
#7715=EDGE_CURVE('',#6482,#6482,#5628,.T.);
#7716=EDGE_CURVE('',#6481,#6483,#4209,.T.);
#7717=EDGE_CURVE('',#6483,#6483,#5629,.T.);
#7718=EDGE_CURVE('',#6484,#6484,#5630,.T.);
#7719=EDGE_CURVE('',#6484,#6482,#4210,.T.);
#7720=EDGE_CURVE('',#6485,#6485,#5631,.T.);
#7721=EDGE_CURVE('',#6485,#6486,#4211,.T.);
#7722=EDGE_CURVE('',#6486,#6486,#5632,.T.);
#7723=EDGE_CURVE('',#6487,#6487,#5633,.T.);
#7724=EDGE_CURVE('',#6487,#6488,#4212,.T.);
#7725=EDGE_CURVE('',#6488,#6488,#5634,.T.);
#7726=EDGE_CURVE('',#6489,#6489,#5635,.T.);
#7727=EDGE_CURVE('',#6489,#6490,#4213,.T.);
#7728=EDGE_CURVE('',#6490,#6490,#5636,.T.);
#7729=EDGE_CURVE('',#6491,#6491,#5637,.T.);
#7730=EDGE_CURVE('',#6491,#6492,#4214,.T.);
#7731=EDGE_CURVE('',#6492,#6492,#5638,.T.);
#7732=EDGE_CURVE('',#6493,#6493,#5639,.T.);
#7733=EDGE_CURVE('',#6493,#6494,#4215,.T.);
#7734=EDGE_CURVE('',#6494,#6494,#5640,.T.);
#7735=EDGE_CURVE('',#6495,#6495,#5641,.T.);
#7736=EDGE_CURVE('',#6495,#6496,#4216,.T.);
#7737=EDGE_CURVE('',#6496,#6496,#5642,.T.);
#7738=EDGE_CURVE('',#6497,#6497,#5643,.T.);
#7739=EDGE_CURVE('',#6498,#6498,#5644,.T.);
#7740=EDGE_CURVE('',#6499,#6499,#5645,.T.);
#7741=EDGE_CURVE('',#6499,#6497,#4217,.T.);
#7742=EDGE_CURVE('',#6498,#6500,#4218,.T.);
#7743=EDGE_CURVE('',#6500,#6500,#5646,.T.);
#7744=EDGE_CURVE('',#6501,#6501,#5647,.T.);
#7745=EDGE_CURVE('',#6502,#6502,#5648,.T.);
#7746=EDGE_CURVE('',#6503,#6503,#5649,.T.);
#7747=EDGE_CURVE('',#6503,#6501,#4219,.T.);
#7748=EDGE_CURVE('',#6502,#6504,#4220,.T.);
#7749=EDGE_CURVE('',#6504,#6504,#5650,.T.);
#7750=EDGE_CURVE('',#6505,#6505,#5651,.T.);
#7751=EDGE_CURVE('',#6506,#6506,#5652,.T.);
#7752=EDGE_CURVE('',#6507,#6507,#5653,.T.);
#7753=EDGE_CURVE('',#6507,#6505,#4221,.T.);
#7754=EDGE_CURVE('',#6506,#6508,#4222,.T.);
#7755=EDGE_CURVE('',#6508,#6508,#5654,.T.);
#7756=EDGE_CURVE('',#6509,#6509,#5655,.T.);
#7757=EDGE_CURVE('',#6510,#6510,#5656,.T.);
#7758=EDGE_CURVE('',#6511,#6511,#5657,.T.);
#7759=EDGE_CURVE('',#6511,#6509,#4223,.T.);
#7760=EDGE_CURVE('',#6510,#6512,#4224,.T.);
#7761=EDGE_CURVE('',#6512,#6512,#5658,.T.);
#7762=EDGE_CURVE('',#6513,#6513,#5659,.T.);
#7763=EDGE_CURVE('',#6513,#6514,#4225,.T.);
#7764=EDGE_CURVE('',#6514,#6514,#5660,.T.);
#7765=EDGE_CURVE('',#6515,#6515,#5661,.T.);
#7766=EDGE_CURVE('',#6515,#6516,#4226,.T.);
#7767=EDGE_CURVE('',#6516,#6516,#5662,.T.);
#7768=EDGE_CURVE('',#6517,#6517,#5663,.T.);
#7769=EDGE_CURVE('',#6517,#6518,#4227,.T.);
#7770=EDGE_CURVE('',#6518,#6518,#5664,.T.);
#7771=EDGE_CURVE('',#6519,#6519,#5665,.T.);
#7772=EDGE_CURVE('',#6519,#6520,#4228,.T.);
#7773=EDGE_CURVE('',#6520,#6520,#5666,.T.);
#7774=EDGE_CURVE('',#6521,#6521,#5667,.T.);
#7775=EDGE_CURVE('',#6521,#6522,#4229,.T.);
#7776=EDGE_CURVE('',#6522,#6522,#5668,.T.);
#7777=EDGE_CURVE('',#6523,#6523,#5669,.T.);
#7778=EDGE_CURVE('',#6523,#6524,#4230,.T.);
#7779=EDGE_CURVE('',#6524,#6524,#5670,.T.);
#7780=EDGE_CURVE('',#6525,#6525,#5671,.T.);
#7781=EDGE_CURVE('',#6526,#6526,#5672,.T.);
#7782=EDGE_CURVE('',#6525,#6527,#4231,.T.);
#7783=EDGE_CURVE('',#6527,#6527,#5673,.T.);
#7784=EDGE_CURVE('',#6528,#6528,#5674,.T.);
#7785=EDGE_CURVE('',#6528,#6526,#4232,.T.);
#7786=EDGE_CURVE('',#6529,#6529,#5675,.T.);
#7787=EDGE_CURVE('',#6530,#6530,#5676,.T.);
#7788=EDGE_CURVE('',#6529,#6531,#4233,.T.);
#7789=EDGE_CURVE('',#6531,#6531,#5677,.T.);
#7790=EDGE_CURVE('',#6532,#6532,#5678,.T.);
#7791=EDGE_CURVE('',#6532,#6530,#4234,.T.);
#7792=EDGE_CURVE('',#6533,#6533,#5679,.T.);
#7793=EDGE_CURVE('',#6534,#6534,#5680,.T.);
#7794=EDGE_CURVE('',#6533,#6535,#4235,.T.);
#7795=EDGE_CURVE('',#6535,#6535,#5681,.T.);
#7796=EDGE_CURVE('',#6536,#6536,#5682,.T.);
#7797=EDGE_CURVE('',#6536,#6534,#4236,.T.);
#7798=EDGE_CURVE('',#6537,#6537,#5683,.T.);
#7799=EDGE_CURVE('',#6538,#6538,#5684,.T.);
#7800=EDGE_CURVE('',#6537,#6539,#4237,.T.);
#7801=EDGE_CURVE('',#6539,#6539,#5685,.T.);
#7802=EDGE_CURVE('',#6540,#6540,#5686,.T.);
#7803=EDGE_CURVE('',#6540,#6538,#4238,.T.);
#7804=EDGE_CURVE('',#6541,#6541,#5687,.T.);
#7805=EDGE_CURVE('',#6541,#6542,#4239,.T.);
#7806=EDGE_CURVE('',#6542,#6542,#5688,.T.);
#7807=EDGE_CURVE('',#6543,#6543,#5689,.T.);
#7808=EDGE_CURVE('',#6543,#6544,#4240,.T.);
#7809=EDGE_CURVE('',#6544,#6544,#5690,.T.);
#7810=EDGE_CURVE('',#6545,#6545,#5691,.T.);
#7811=EDGE_CURVE('',#6545,#6546,#4241,.T.);
#7812=EDGE_CURVE('',#6546,#6546,#5692,.T.);
#7813=EDGE_CURVE('',#6547,#6547,#5693,.T.);
#7814=EDGE_CURVE('',#6547,#6548,#4242,.T.);
#7815=EDGE_CURVE('',#6548,#6548,#5694,.T.);
#7816=EDGE_CURVE('',#6549,#6549,#5695,.T.);
#7817=EDGE_CURVE('',#6549,#6550,#4243,.T.);
#7818=EDGE_CURVE('',#6550,#6550,#5696,.T.);
#7819=EDGE_CURVE('',#6551,#6551,#5697,.T.);
#7820=EDGE_CURVE('',#6551,#6552,#4244,.T.);
#7821=EDGE_CURVE('',#6552,#6552,#5698,.T.);
#7822=EDGE_CURVE('',#6553,#6553,#5699,.T.);
#7823=EDGE_CURVE('',#6554,#6554,#5700,.T.);
#7824=EDGE_CURVE('',#6555,#6555,#5701,.T.);
#7825=EDGE_CURVE('',#6555,#6553,#4245,.T.);
#7826=EDGE_CURVE('',#6554,#6556,#4246,.T.);
#7827=EDGE_CURVE('',#6556,#6556,#5702,.T.);
#7828=EDGE_CURVE('',#6557,#6557,#5703,.T.);
#7829=EDGE_CURVE('',#6558,#6558,#5704,.T.);
#7830=EDGE_CURVE('',#6559,#6559,#5705,.T.);
#7831=EDGE_CURVE('',#6559,#6557,#4247,.T.);
#7832=EDGE_CURVE('',#6558,#6560,#4248,.T.);
#7833=EDGE_CURVE('',#6560,#6560,#5706,.T.);
#7834=EDGE_CURVE('',#6561,#6561,#5707,.T.);
#7835=EDGE_CURVE('',#6562,#6562,#5708,.T.);
#7836=EDGE_CURVE('',#6563,#6563,#5709,.T.);
#7837=EDGE_CURVE('',#6563,#6561,#4249,.T.);
#7838=EDGE_CURVE('',#6562,#6564,#4250,.T.);
#7839=EDGE_CURVE('',#6564,#6564,#5710,.T.);
#7840=EDGE_CURVE('',#6565,#6565,#5711,.T.);
#7841=EDGE_CURVE('',#6566,#6566,#5712,.T.);
#7842=EDGE_CURVE('',#6567,#6567,#5713,.T.);
#7843=EDGE_CURVE('',#6567,#6565,#4251,.T.);
#7844=EDGE_CURVE('',#6566,#6568,#4252,.T.);
#7845=EDGE_CURVE('',#6568,#6568,#5714,.T.);
#7846=EDGE_CURVE('',#6569,#6570,#5715,.T.);
#7847=EDGE_CURVE('',#6570,#6569,#5716,.T.);
#7848=EDGE_CURVE('',#6570,#6571,#5717,.T.);
#7849=EDGE_CURVE('',#6572,#6571,#5718,.T.);
#7850=EDGE_CURVE('',#6571,#6572,#5719,.T.);
#7851=EDGE_CURVE('',#6572,#6573,#4253,.T.);
#7852=EDGE_CURVE('',#6573,#6573,#5720,.T.);
#7853=EDGE_CURVE('',#6574,#6574,#5721,.T.);
#7854=EDGE_CURVE('',#6574,#6575,#4254,.T.);
#7855=EDGE_CURVE('',#6575,#6575,#5722,.T.);
#7856=EDGE_CURVE('',#6575,#6576,#4255,.T.);
#7857=EDGE_CURVE('',#6576,#6576,#5723,.T.);
#7858=EDGE_CURVE('',#6577,#6577,#5724,.T.);
#7859=EDGE_CURVE('',#6577,#6569,#4256,.T.);
#7860=EDGE_CURVE('',#6578,#6578,#5725,.T.);
#7861=EDGE_CURVE('',#6578,#6574,#4257,.T.);
#7862=EDGE_CURVE('',#6579,#6580,#5726,.T.);
#7863=EDGE_CURVE('',#6580,#6579,#5727,.T.);
#7864=EDGE_CURVE('',#6580,#6581,#5728,.T.);
#7865=EDGE_CURVE('',#6582,#6581,#5729,.T.);
#7866=EDGE_CURVE('',#6581,#6582,#5730,.T.);
#7867=EDGE_CURVE('',#6583,#6583,#5731,.T.);
#7868=EDGE_CURVE('',#6583,#6582,#4258,.T.);
#7869=EDGE_CURVE('',#6584,#6584,#5732,.T.);
#7870=EDGE_CURVE('',#6585,#6585,#5733,.T.);
#7871=EDGE_CURVE('',#6586,#6586,#5734,.T.);
#7872=EDGE_CURVE('',#6586,#6584,#4259,.T.);
#7873=EDGE_CURVE('',#6587,#6587,#5735,.T.);
#7874=EDGE_CURVE('',#6587,#6586,#4260,.T.);
#7875=EDGE_CURVE('',#6588,#6588,#5736,.T.);
#7876=EDGE_CURVE('',#6588,#6587,#4261,.T.);
#7877=EDGE_CURVE('',#6579,#6585,#4262,.T.);
#7878=EDGE_CURVE('',#6589,#6590,#5737,.T.);
#7879=EDGE_CURVE('',#6591,#6592,#5738,.T.);
#7880=EDGE_CURVE('',#6593,#6594,#5739,.T.);
#7881=EDGE_CURVE('',#6595,#6596,#5740,.T.);
#7882=EDGE_CURVE('',#6597,#6598,#5741,.T.);
#7883=EDGE_CURVE('',#6599,#6600,#5742,.T.);
#7884=EDGE_CURVE('',#6601,#6602,#5743,.T.);
#7885=EDGE_CURVE('',#6603,#6604,#599,.T.);
#7886=EDGE_CURVE('',#6605,#6603,#5744,.T.);
#7887=EDGE_CURVE('',#6606,#6605,#600,.T.);
#7888=EDGE_CURVE('',#6604,#6606,#5745,.T.);
#7889=EDGE_CURVE('',#6607,#6605,#5746,.T.);
#7890=EDGE_CURVE('',#6607,#6608,#601,.T.);
#7891=EDGE_CURVE('',#6609,#6608,#5747,.T.);
#7892=EDGE_CURVE('',#6609,#6610,#602,.T.);
#7893=EDGE_CURVE('',#6611,#6610,#5748,.T.);
#7894=EDGE_CURVE('',#6611,#6612,#4263,.T.);
#7895=EDGE_CURVE('',#6612,#6612,#5749,.T.);
#7896=EDGE_CURVE('',#6613,#6611,#5750,.T.);
#7897=EDGE_CURVE('',#6613,#6614,#603,.T.);
#7898=EDGE_CURVE('',#6615,#6614,#5751,.T.);
#7899=EDGE_CURVE('',#6615,#6616,#604,.T.);
#7900=EDGE_CURVE('',#6617,#6616,#5752,.T.);
#7901=EDGE_CURVE('',#6617,#6618,#605,.T.);
#7902=EDGE_CURVE('',#6619,#6618,#5753,.T.);
#7903=EDGE_CURVE('',#6619,#6620,#606,.T.);
#7904=EDGE_CURVE('',#6606,#6620,#5754,.T.);
#7905=EDGE_CURVE('',#6603,#6621,#5755,.T.);
#7906=EDGE_CURVE('',#6621,#6607,#5756,.T.);
#7907=EDGE_CURVE('',#6622,#6621,#607,.T.);
#7908=EDGE_CURVE('',#6608,#6622,#5757,.T.);
#7909=EDGE_CURVE('',#6622,#6623,#5758,.T.);
#7910=EDGE_CURVE('',#6623,#6609,#5759,.T.);
#7911=EDGE_CURVE('',#6624,#6623,#608,.T.);
#7912=EDGE_CURVE('',#6610,#6624,#5760,.T.);
#7913=EDGE_CURVE('',#6624,#6625,#5761,.T.);
#7914=EDGE_CURVE('',#6625,#6626,#5762,.T.);
#7915=EDGE_CURVE('',#6626,#6613,#5763,.T.);
#7916=EDGE_CURVE('',#6627,#6626,#609,.T.);
#7917=EDGE_CURVE('',#6614,#6627,#5764,.T.);
#7918=EDGE_CURVE('',#6627,#6628,#5765,.T.);
#7919=EDGE_CURVE('',#6628,#6615,#5766,.T.);
#7920=EDGE_CURVE('',#6629,#6628,#610,.T.);
#7921=EDGE_CURVE('',#6616,#6629,#5767,.T.);
#7922=EDGE_CURVE('',#6629,#6630,#5768,.T.);
#7923=EDGE_CURVE('',#6630,#6617,#5769,.T.);
#7924=EDGE_CURVE('',#6631,#6630,#611,.T.);
#7925=EDGE_CURVE('',#6618,#6631,#5770,.T.);
#7926=EDGE_CURVE('',#6632,#6632,#5771,.T.);
#7927=EDGE_CURVE('',#6632,#6625,#4264,.T.);
#7928=EDGE_CURVE('',#6633,#6604,#5772,.T.);
#7929=EDGE_CURVE('',#6633,#6634,#612,.T.);
#7930=EDGE_CURVE('',#6631,#6634,#5773,.T.);
#7931=EDGE_CURVE('',#6620,#6633,#5774,.T.);
#7932=EDGE_CURVE('',#6634,#6619,#5775,.T.);
#7933=EDGE_CURVE('',#6635,#6635,#5776,.T.);
#7934=EDGE_CURVE('',#6636,#6636,#5777,.T.);
#7935=EDGE_CURVE('',#6637,#6637,#5778,.T.);
#7936=EDGE_CURVE('',#6637,#6635,#4265,.T.);
#7937=EDGE_CURVE('',#6638,#6638,#5779,.T.);
#7938=EDGE_CURVE('',#6638,#6636,#4266,.T.);
#7939=EDGE_CURVE('',#6639,#6639,#5780,.T.);
#7940=EDGE_CURVE('',#6640,#6640,#5781,.T.);
#7941=EDGE_CURVE('',#6641,#6641,#5782,.T.);
#7942=EDGE_CURVE('',#6641,#6639,#4267,.T.);
#7943=EDGE_CURVE('',#6642,#6642,#5783,.T.);
#7944=EDGE_CURVE('',#6642,#6640,#4268,.T.);
#7945=EDGE_CURVE('',#6643,#6643,#5784,.T.);
#7946=EDGE_CURVE('',#6643,#6644,#4269,.T.);
#7947=EDGE_CURVE('',#6644,#6644,#5785,.T.);
#7948=EDGE_CURVE('',#6645,#6645,#5786,.T.);
#7949=EDGE_CURVE('',#6645,#6646,#4270,.T.);
#7950=EDGE_CURVE('',#6646,#6646,#5787,.T.);
#7951=EDGE_CURVE('',#6647,#6647,#5788,.T.);
#7952=EDGE_CURVE('',#6647,#6648,#4271,.T.);
#7953=EDGE_CURVE('',#6648,#6648,#5789,.T.);
#7954=EDGE_CURVE('',#6649,#6649,#5790,.T.);
#7955=EDGE_CURVE('',#6649,#6650,#4272,.T.);
#7956=EDGE_CURVE('',#6650,#6650,#5791,.T.);
#7957=EDGE_CURVE('',#6651,#6651,#5792,.T.);
#7958=EDGE_CURVE('',#6651,#6652,#4273,.T.);
#7959=EDGE_CURVE('',#6652,#6652,#5793,.T.);
#7960=EDGE_CURVE('',#6653,#6653,#5794,.T.);
#7961=EDGE_CURVE('',#6653,#6654,#4274,.T.);
#7962=EDGE_CURVE('',#6654,#6654,#5795,.T.);
#7963=EDGE_CURVE('',#6655,#6655,#5796,.T.);
#7964=EDGE_CURVE('',#6655,#6656,#4275,.T.);
#7965=EDGE_CURVE('',#6656,#6656,#5797,.T.);
#7966=EDGE_CURVE('',#6657,#6657,#5798,.T.);
#7967=EDGE_CURVE('',#6657,#6658,#4276,.T.);
#7968=EDGE_CURVE('',#6658,#6658,#5799,.T.);
#7969=EDGE_CURVE('',#6659,#6660,#4277,.T.);
#7970=EDGE_CURVE('',#6661,#6659,#4278,.T.);
#7971=EDGE_CURVE('',#6661,#6662,#4279,.T.);
#7972=EDGE_CURVE('',#6660,#6662,#4280,.T.);
#7973=EDGE_CURVE('',#6663,#6664,#4281,.T.);
#7974=EDGE_CURVE('',#6665,#6663,#4282,.T.);
#7975=EDGE_CURVE('',#6666,#6665,#4283,.T.);
#7976=EDGE_CURVE('',#6664,#6666,#4284,.T.);
#7977=EDGE_CURVE('',#6666,#6661,#4285,.T.);
#7978=EDGE_CURVE('',#6662,#6665,#4286,.T.);
#7979=EDGE_CURVE('',#6667,#6660,#5800,.T.);
#7980=EDGE_CURVE('',#6668,#6667,#4287,.T.);
#7981=EDGE_CURVE('',#6668,#6659,#5801,.T.);
#7982=EDGE_CURVE('',#6664,#6669,#5802,.T.);
#7983=EDGE_CURVE('',#6670,#6669,#4288,.T.);
#7984=EDGE_CURVE('',#6663,#6670,#5803,.T.);
#7985=EDGE_CURVE('',#6671,#6668,#4289,.T.);
#7986=EDGE_CURVE('',#6671,#6672,#4290,.T.);
#7987=EDGE_CURVE('',#6672,#6673,#4291,.T.);
#7988=EDGE_CURVE('',#6673,#6674,#4292,.T.);
#7989=EDGE_CURVE('',#6675,#6674,#5804,.T.);
#7990=EDGE_CURVE('',#6669,#6675,#4293,.T.);
#7991=EDGE_CURVE('',#6674,#6676,#4294,.T.);
#7992=EDGE_CURVE('',#6673,#6677,#4295,.T.);
#7993=EDGE_CURVE('',#6676,#6677,#4296,.T.);
#7994=EDGE_CURVE('',#6678,#6671,#4297,.T.);
#7995=EDGE_CURVE('',#6679,#6678,#4298,.T.);
#7996=EDGE_CURVE('',#6672,#6679,#4299,.T.);
#7997=EDGE_CURVE('',#6677,#6679,#4300,.T.);
#7998=EDGE_CURVE('',#6678,#6667,#4301,.T.);
#7999=EDGE_CURVE('',#6680,#6676,#5805,.T.);
#8000=EDGE_CURVE('',#6675,#6680,#4302,.T.);
#8001=EDGE_CURVE('',#6670,#6680,#4303,.T.);
#8002=EDGE_CURVE('',#6681,#6682,#4304,.T.);
#8003=EDGE_CURVE('',#6682,#6683,#4305,.T.);
#8004=EDGE_CURVE('',#6684,#6683,#4306,.T.);
#8005=EDGE_CURVE('',#6681,#6684,#4307,.T.);
#8006=EDGE_CURVE('',#6685,#6681,#4308,.T.);
#8007=EDGE_CURVE('',#6686,#6684,#4309,.T.);
#8008=EDGE_CURVE('',#6685,#6686,#4310,.T.);
#8009=EDGE_CURVE('',#6687,#6685,#4311,.T.);
#8010=EDGE_CURVE('',#6688,#6686,#4312,.T.);
#8011=EDGE_CURVE('',#6687,#6688,#4313,.T.);
#8012=EDGE_CURVE('',#6682,#6687,#4314,.T.);
#8013=EDGE_CURVE('',#6683,#6688,#4315,.T.);
#8014=EDGE_CURVE('',#6689,#6690,#4316,.T.);
#8015=EDGE_CURVE('',#6690,#6691,#4317,.T.);
#8016=EDGE_CURVE('',#6692,#6691,#4318,.T.);
#8017=EDGE_CURVE('',#6689,#6692,#4319,.T.);
#8018=EDGE_CURVE('',#6693,#6689,#4320,.T.);
#8019=EDGE_CURVE('',#6694,#6692,#4321,.T.);
#8020=EDGE_CURVE('',#6693,#6694,#4322,.T.);
#8021=EDGE_CURVE('',#6695,#6693,#4323,.T.);
#8022=EDGE_CURVE('',#6696,#6694,#4324,.T.);
#8023=EDGE_CURVE('',#6695,#6696,#4325,.T.);
#8024=EDGE_CURVE('',#6690,#6695,#4326,.T.);
#8025=EDGE_CURVE('',#6691,#6696,#4327,.T.);
#8026=EDGE_CURVE('',#6697,#6698,#4328,.T.);
#8027=EDGE_CURVE('',#6698,#6699,#4329,.T.);
#8028=EDGE_CURVE('',#6700,#6699,#4330,.T.);
#8029=EDGE_CURVE('',#6697,#6700,#4331,.T.);
#8030=EDGE_CURVE('',#6701,#6697,#4332,.T.);
#8031=EDGE_CURVE('',#6702,#6700,#4333,.T.);
#8032=EDGE_CURVE('',#6701,#6702,#4334,.T.);
#8033=EDGE_CURVE('',#6703,#6701,#4335,.T.);
#8034=EDGE_CURVE('',#6704,#6702,#4336,.T.);
#8035=EDGE_CURVE('',#6703,#6704,#4337,.T.);
#8036=EDGE_CURVE('',#6698,#6703,#4338,.T.);
#8037=EDGE_CURVE('',#6699,#6704,#4339,.T.);
#8038=EDGE_CURVE('',#6705,#6705,#5806,.T.);
#8039=EDGE_CURVE('',#6705,#6706,#4340,.T.);
#8040=EDGE_CURVE('',#6706,#6706,#5807,.T.);
#8041=EDGE_CURVE('',#6707,#6707,#5808,.T.);
#8042=EDGE_CURVE('',#6707,#6708,#4341,.T.);
#8043=EDGE_CURVE('',#6708,#6708,#5809,.T.);
#8044=EDGE_CURVE('',#6709,#6709,#5810,.T.);
#8045=EDGE_CURVE('',#6709,#6710,#4342,.T.);
#8046=EDGE_CURVE('',#6710,#6710,#5811,.T.);
#8047=EDGE_CURVE('',#6711,#6711,#5812,.T.);
#8048=EDGE_CURVE('',#6711,#6712,#4343,.T.);
#8049=EDGE_CURVE('',#6712,#6712,#5813,.T.);
#8050=EDGE_CURVE('',#6713,#6713,#5814,.T.);
#8051=EDGE_CURVE('',#6714,#6714,#5815,.T.);
#8052=EDGE_CURVE('',#6715,#6715,#5816,.T.);
#8053=EDGE_CURVE('',#6716,#6716,#5817,.T.);
#8054=EDGE_CURVE('',#6713,#6715,#4344,.T.);
#8055=EDGE_CURVE('',#6716,#6717,#4345,.T.);
#8056=EDGE_CURVE('',#6717,#6717,#5818,.T.);
#8057=EDGE_CURVE('',#6718,#6718,#5819,.T.);
#8058=EDGE_CURVE('',#6718,#6714,#4346,.T.);
#8059=EDGE_CURVE('',#6719,#6719,#5820,.T.);
#8060=EDGE_CURVE('',#6719,#6720,#4347,.T.);
#8061=EDGE_CURVE('',#6720,#6720,#5821,.T.);
#8062=EDGE_CURVE('',#6721,#6721,#5822,.T.);
#8063=EDGE_CURVE('',#6721,#6722,#4348,.T.);
#8064=EDGE_CURVE('',#6722,#6722,#5823,.T.);
#8065=EDGE_CURVE('',#6723,#6723,#5824,.T.);
#8066=EDGE_CURVE('',#6723,#6724,#4349,.T.);
#8067=EDGE_CURVE('',#6724,#6724,#5825,.T.);
#8068=EDGE_CURVE('',#6725,#6725,#5826,.T.);
#8069=EDGE_CURVE('',#6725,#6726,#4350,.T.);
#8070=EDGE_CURVE('',#6726,#6726,#5827,.T.);
#8071=EDGE_CURVE('',#6727,#6727,#5828,.T.);
#8072=EDGE_CURVE('',#6727,#6728,#4351,.T.);
#8073=EDGE_CURVE('',#6728,#6728,#5829,.T.);
#8074=EDGE_CURVE('',#6729,#6729,#5830,.T.);
#8075=EDGE_CURVE('',#6729,#6730,#4352,.T.);
#8076=EDGE_CURVE('',#6730,#6730,#5831,.T.);
#8077=EDGE_CURVE('',#6731,#6731,#5832,.T.);
#8078=EDGE_CURVE('',#6731,#6732,#4353,.T.);
#8079=EDGE_CURVE('',#6732,#6732,#5833,.T.);
#8080=EDGE_CURVE('',#6733,#6733,#5834,.T.);
#8081=EDGE_CURVE('',#6733,#6734,#4354,.T.);
#8082=EDGE_CURVE('',#6734,#6734,#5835,.T.);
#8083=EDGE_CURVE('',#6735,#6735,#5836,.T.);
#8084=EDGE_CURVE('',#6735,#6736,#4355,.T.);
#8085=EDGE_CURVE('',#6736,#6736,#5837,.T.);
#8086=EDGE_CURVE('',#6737,#6737,#5838,.T.);
#8087=EDGE_CURVE('',#6737,#6738,#4356,.T.);
#8088=EDGE_CURVE('',#6738,#6738,#5839,.T.);
#8089=EDGE_CURVE('',#6739,#6739,#5840,.T.);
#8090=EDGE_CURVE('',#6739,#6740,#4357,.T.);
#8091=EDGE_CURVE('',#6740,#6740,#5841,.T.);
#8092=EDGE_CURVE('',#6741,#6741,#5842,.T.);
#8093=EDGE_CURVE('',#6741,#6742,#4358,.T.);
#8094=EDGE_CURVE('',#6742,#6742,#5843,.T.);
#8095=EDGE_CURVE('',#6743,#6743,#5844,.T.);
#8096=EDGE_CURVE('',#6744,#6744,#5845,.T.);
#8097=EDGE_CURVE('',#6745,#6745,#5846,.T.);
#8098=EDGE_CURVE('',#6746,#6746,#5847,.T.);
#8099=EDGE_CURVE('',#6743,#6745,#4359,.T.);
#8100=EDGE_CURVE('',#6746,#6747,#4360,.T.);
#8101=EDGE_CURVE('',#6747,#6747,#5848,.T.);
#8102=EDGE_CURVE('',#6748,#6748,#5849,.T.);
#8103=EDGE_CURVE('',#6748,#6744,#4361,.T.);
#8104=EDGE_CURVE('',#6749,#6749,#5850,.T.);
#8105=EDGE_CURVE('',#6749,#6750,#4362,.T.);
#8106=EDGE_CURVE('',#6750,#6750,#5851,.T.);
#8107=EDGE_CURVE('',#6751,#6751,#5852,.T.);
#8108=EDGE_CURVE('',#6751,#6752,#4363,.T.);
#8109=EDGE_CURVE('',#6752,#6752,#5853,.T.);
#8110=EDGE_CURVE('',#6753,#6753,#5854,.T.);
#8111=EDGE_CURVE('',#6753,#6754,#4364,.T.);
#8112=EDGE_CURVE('',#6754,#6754,#5855,.T.);
#8113=EDGE_CURVE('',#6755,#6755,#5856,.T.);
#8114=EDGE_CURVE('',#6755,#6756,#4365,.T.);
#8115=EDGE_CURVE('',#6756,#6756,#5857,.T.);
#8116=EDGE_CURVE('',#6757,#6757,#5858,.T.);
#8117=EDGE_CURVE('',#6757,#6758,#4366,.T.);
#8118=EDGE_CURVE('',#6758,#6758,#5859,.T.);
#8119=EDGE_CURVE('',#6759,#6759,#5860,.T.);
#8120=EDGE_CURVE('',#6759,#6760,#4367,.T.);
#8121=EDGE_CURVE('',#6760,#6760,#5861,.T.);
#8122=EDGE_CURVE('',#6761,#6761,#5862,.T.);
#8123=EDGE_CURVE('',#6762,#6762,#5863,.T.);
#8124=EDGE_CURVE('',#6762,#6761,#4368,.T.);
#8125=EDGE_CURVE('',#6763,#6763,#5864,.T.);
#8126=EDGE_CURVE('',#6763,#6762,#4369,.T.);
#8127=EDGE_CURVE('',#6764,#6764,#5865,.T.);
#8128=EDGE_CURVE('',#6764,#6763,#4370,.T.);
#8129=EDGE_CURVE('',#6765,#6765,#5866,.T.);
#8130=EDGE_CURVE('',#6766,#6766,#5867,.F.);
#8131=EDGE_CURVE('',#6766,#6765,#4371,.T.);
#8132=EDGE_CURVE('',#6767,#6767,#5868,.F.);
#8133=EDGE_CURVE('',#6767,#6766,#4372,.T.);
#8134=EDGE_CURVE('',#6768,#6768,#5869,.T.);
#8135=EDGE_CURVE('',#6768,#6767,#4373,.T.);
#8136=EDGE_CURVE('',#6769,#6770,#4374,.T.);
#8137=EDGE_CURVE('',#6770,#6771,#4375,.T.);
#8138=EDGE_CURVE('',#6771,#6772,#4376,.T.);
#8139=EDGE_CURVE('',#6769,#6772,#4377,.T.);
#8140=EDGE_CURVE('',#6770,#6773,#4378,.T.);
#8141=EDGE_CURVE('',#6773,#6774,#4379,.T.);
#8142=EDGE_CURVE('',#6774,#6771,#4380,.T.);
#8143=EDGE_CURVE('',#6773,#6775,#4381,.T.);
#8144=EDGE_CURVE('',#6775,#6776,#4382,.T.);
#8145=EDGE_CURVE('',#6776,#6774,#4383,.T.);
#8146=EDGE_CURVE('',#6775,#6777,#4384,.T.);
#8147=EDGE_CURVE('',#6777,#6778,#4385,.T.);
#8148=EDGE_CURVE('',#6778,#6776,#4386,.T.);
#8149=EDGE_CURVE('',#6777,#6779,#4387,.T.);
#8150=EDGE_CURVE('',#6779,#6780,#4388,.T.);
#8151=EDGE_CURVE('',#6780,#6778,#4389,.T.);
#8152=EDGE_CURVE('',#6779,#6769,#4390,.T.);
#8153=EDGE_CURVE('',#6772,#6780,#4391,.T.);
#8154=EDGE_CURVE('',#6781,#6781,#5870,.T.);
#8155=EDGE_CURVE('',#6781,#6782,#4392,.T.);
#8156=EDGE_CURVE('',#6782,#6782,#5871,.T.);
#8157=EDGE_CURVE('',#6783,#6783,#5872,.T.);
#8158=EDGE_CURVE('',#6783,#6784,#4393,.T.);
#8159=EDGE_CURVE('',#6784,#6784,#5873,.T.);
#8160=EDGE_CURVE('',#6785,#6785,#5874,.T.);
#8161=EDGE_CURVE('',#6785,#6786,#4394,.T.);
#8162=EDGE_CURVE('',#6786,#6786,#5875,.T.);
#8163=EDGE_CURVE('',#6787,#6788,#4395,.T.);
#8164=EDGE_CURVE('',#6788,#6789,#4396,.T.);
#8165=EDGE_CURVE('',#6790,#6789,#4397,.T.);
#8166=EDGE_CURVE('',#6787,#6790,#4398,.T.);
#8167=EDGE_CURVE('',#6791,#6787,#4399,.T.);
#8168=EDGE_CURVE('',#6792,#6790,#4400,.T.);
#8169=EDGE_CURVE('',#6791,#6792,#4401,.T.);
#8170=EDGE_CURVE('',#6793,#6791,#4402,.T.);
#8171=EDGE_CURVE('',#6794,#6792,#4403,.T.);
#8172=EDGE_CURVE('',#6793,#6794,#4404,.T.);
#8173=EDGE_CURVE('',#6788,#6793,#4405,.T.);
#8174=EDGE_CURVE('',#6789,#6794,#4406,.T.);
#8175=EDGE_CURVE('',#6795,#6795,#5876,.T.);
#8176=EDGE_CURVE('',#6795,#6796,#4407,.T.);
#8177=EDGE_CURVE('',#6796,#6796,#5877,.T.);
#8178=EDGE_CURVE('',#6797,#6797,#5878,.T.);
#8179=EDGE_CURVE('',#6797,#6798,#4408,.T.);
#8180=EDGE_CURVE('',#6798,#6798,#5879,.T.);
#8181=EDGE_CURVE('',#6799,#6799,#5880,.T.);
#8182=EDGE_CURVE('',#6799,#6800,#4409,.T.);
#8183=EDGE_CURVE('',#6800,#6800,#5881,.T.);
#8184=EDGE_CURVE('',#6801,#6802,#4410,.T.);
#8185=EDGE_CURVE('',#6802,#6803,#4411,.T.);
#8186=EDGE_CURVE('',#6804,#6803,#4412,.T.);
#8187=EDGE_CURVE('',#6801,#6804,#4413,.T.);
#8188=EDGE_CURVE('',#6805,#6801,#4414,.T.);
#8189=EDGE_CURVE('',#6806,#6804,#4415,.T.);
#8190=EDGE_CURVE('',#6805,#6806,#4416,.T.);
#8191=EDGE_CURVE('',#6807,#6805,#4417,.T.);
#8192=EDGE_CURVE('',#6808,#6806,#4418,.T.);
#8193=EDGE_CURVE('',#6807,#6808,#4419,.T.);
#8194=EDGE_CURVE('',#6802,#6807,#4420,.T.);
#8195=EDGE_CURVE('',#6803,#6808,#4421,.T.);
#8196=EDGE_CURVE('',#6809,#6809,#5882,.T.);
#8197=EDGE_CURVE('',#6809,#6810,#4422,.T.);
#8198=EDGE_CURVE('',#6810,#6810,#5883,.T.);
#8199=EDGE_CURVE('',#6811,#6811,#5884,.T.);
#8200=EDGE_CURVE('',#6811,#6812,#4423,.T.);
#8201=EDGE_CURVE('',#6812,#6812,#5885,.T.);
#8202=EDGE_CURVE('',#6813,#6813,#5886,.T.);
#8203=EDGE_CURVE('',#6813,#6814,#4424,.T.);
#8204=EDGE_CURVE('',#6814,#6814,#5887,.T.);
#8205=EDGE_CURVE('',#6815,#6816,#4425,.T.);
#8206=EDGE_CURVE('',#6816,#6817,#4426,.T.);
#8207=EDGE_CURVE('',#6818,#6817,#4427,.T.);
#8208=EDGE_CURVE('',#6815,#6818,#4428,.T.);
#8209=EDGE_CURVE('',#6819,#6815,#4429,.T.);
#8210=EDGE_CURVE('',#6820,#6818,#4430,.T.);
#8211=EDGE_CURVE('',#6819,#6820,#4431,.T.);
#8212=EDGE_CURVE('',#6821,#6819,#4432,.T.);
#8213=EDGE_CURVE('',#6822,#6820,#4433,.T.);
#8214=EDGE_CURVE('',#6821,#6822,#4434,.T.);
#8215=EDGE_CURVE('',#6816,#6821,#4435,.T.);
#8216=EDGE_CURVE('',#6817,#6822,#4436,.T.);
#8217=EDGE_CURVE('',#6823,#6823,#5888,.T.);
#8218=EDGE_CURVE('',#6823,#6824,#4437,.T.);
#8219=EDGE_CURVE('',#6824,#6824,#5889,.T.);
#8220=EDGE_CURVE('',#6825,#6826,#4438,.T.);
#8221=EDGE_CURVE('',#6826,#6827,#4439,.T.);
#8222=EDGE_CURVE('',#6828,#6827,#4440,.T.);
#8223=EDGE_CURVE('',#6825,#6828,#4441,.T.);
#8224=EDGE_CURVE('',#6829,#6825,#4442,.T.);
#8225=EDGE_CURVE('',#6830,#6828,#4443,.T.);
#8226=EDGE_CURVE('',#6829,#6830,#4444,.T.);
#8227=EDGE_CURVE('',#6831,#6829,#4445,.T.);
#8228=EDGE_CURVE('',#6832,#6830,#4446,.T.);
#8229=EDGE_CURVE('',#6831,#6832,#4447,.T.);
#8230=EDGE_CURVE('',#6826,#6831,#4448,.T.);
#8231=EDGE_CURVE('',#6827,#6832,#4449,.T.);
#8232=EDGE_CURVE('',#6833,#6833,#5890,.T.);
#8233=EDGE_CURVE('',#6833,#6834,#4450,.T.);
#8234=EDGE_CURVE('',#6834,#6834,#5891,.T.);
#8235=EDGE_CURVE('',#6835,#6835,#5892,.T.);
#8236=EDGE_CURVE('',#6836,#6836,#5893,.T.);
#8237=EDGE_CURVE('',#6835,#6837,#4451,.T.);
#8238=EDGE_CURVE('',#6837,#6837,#5894,.T.);
#8239=EDGE_CURVE('',#6838,#6838,#5895,.T.);
#8240=EDGE_CURVE('',#6838,#6836,#4452,.T.);
#8241=EDGE_CURVE('',#6839,#6839,#5896,.T.);
#8242=EDGE_CURVE('',#6839,#6840,#4453,.T.);
#8243=EDGE_CURVE('',#6840,#6840,#5897,.T.);
#8244=EDGE_CURVE('',#6841,#6841,#5898,.T.);
#8245=EDGE_CURVE('',#6841,#6842,#4454,.T.);
#8246=EDGE_CURVE('',#6842,#6842,#5899,.T.);
#8247=EDGE_CURVE('',#6843,#6843,#5900,.T.);
#8248=EDGE_CURVE('',#6843,#6844,#4455,.T.);
#8249=EDGE_CURVE('',#6844,#6844,#5901,.T.);
#8250=EDGE_CURVE('',#6845,#6845,#5902,.T.);
#8251=EDGE_CURVE('',#6845,#6846,#4456,.T.);
#8252=EDGE_CURVE('',#6846,#6846,#5903,.T.);
#8253=EDGE_CURVE('',#6847,#6848,#5904,.T.);
#8254=EDGE_CURVE('',#6849,#6847,#4457,.T.);
#8255=EDGE_CURVE('',#6850,#6849,#4458,.T.);
#8256=EDGE_CURVE('',#6848,#6850,#4459,.T.);
#8257=EDGE_CURVE('',#6848,#6851,#4460,.T.);
#8258=EDGE_CURVE('',#6852,#6850,#4461,.T.);
#8259=EDGE_CURVE('',#6852,#6851,#4462,.T.);
#8260=EDGE_CURVE('',#6851,#6853,#5905,.T.);
#8261=EDGE_CURVE('',#6854,#6852,#4463,.T.);
#8262=EDGE_CURVE('',#6853,#6854,#4464,.T.);
#8263=EDGE_CURVE('',#6853,#6847,#4465,.T.);
#8264=EDGE_CURVE('',#6854,#6849,#4466,.T.);
#8265=EDGE_CURVE('',#6855,#6855,#5906,.T.);
#8266=EDGE_CURVE('',#6856,#6856,#5907,.T.);
#8267=EDGE_CURVE('',#6857,#6857,#5908,.T.);
#8268=EDGE_CURVE('',#6857,#6855,#4467,.T.);
#8269=EDGE_CURVE('',#6858,#6858,#5909,.T.);
#8270=EDGE_CURVE('',#6859,#6859,#5910,.T.);
#8271=EDGE_CURVE('',#6859,#6858,#4468,.T.);
#8272=EDGE_CURVE('',#6860,#6860,#5911,.T.);
#8273=EDGE_CURVE('',#6861,#6861,#5912,.T.);
#8274=EDGE_CURVE('',#6861,#6860,#4469,.T.);
#8275=EDGE_CURVE('',#6862,#6862,#5913,.T.);
#8276=EDGE_CURVE('',#6863,#6863,#5914,.T.);
#8277=EDGE_CURVE('',#6863,#6862,#4470,.T.);
#8278=EDGE_CURVE('',#6864,#6864,#5915,.T.);
#8279=EDGE_CURVE('',#6865,#6865,#5916,.T.);
#8280=EDGE_CURVE('',#6865,#6864,#4471,.T.);
#8281=EDGE_CURVE('',#6866,#6866,#5917,.T.);
#8282=EDGE_CURVE('',#6866,#6856,#4472,.T.);
#8283=EDGE_CURVE('',#6867,#6868,#5918,.T.);
#8284=EDGE_CURVE('',#6869,#6867,#4473,.T.);
#8285=EDGE_CURVE('',#6870,#6869,#5919,.T.);
#8286=EDGE_CURVE('',#6868,#6870,#4474,.T.);
#8287=EDGE_CURVE('',#6868,#6871,#4475,.T.);
#8288=EDGE_CURVE('',#6872,#6870,#4476,.T.);
#8289=EDGE_CURVE('',#6872,#6871,#4477,.T.);
#8290=EDGE_CURVE('',#6871,#6873,#5920,.T.);
#8291=EDGE_CURVE('',#6874,#6872,#5921,.T.);
#8292=EDGE_CURVE('',#6873,#6874,#4478,.T.);
#8293=EDGE_CURVE('',#6873,#6867,#4479,.T.);
#8294=EDGE_CURVE('',#6869,#6874,#4480,.T.);
#8295=EDGE_CURVE('',#6875,#6875,#5922,.T.);
#8296=EDGE_CURVE('',#6876,#6876,#5923,.T.);
#8297=EDGE_CURVE('',#6877,#6877,#5924,.T.);
#8298=EDGE_CURVE('',#6877,#6875,#4481,.T.);
#8299=EDGE_CURVE('',#6878,#6878,#5925,.T.);
#8300=EDGE_CURVE('',#6878,#6876,#4482,.T.);
#8301=EDGE_CURVE('',#6879,#6880,#4483,.T.);
#8302=EDGE_CURVE('',#6880,#6881,#4484,.T.);
#8303=EDGE_CURVE('',#6881,#6882,#4485,.T.);
#8304=EDGE_CURVE('',#6879,#6882,#4486,.T.);
#8305=EDGE_CURVE('',#6880,#6883,#4487,.T.);
#8306=EDGE_CURVE('',#6883,#6884,#4488,.T.);
#8307=EDGE_CURVE('',#6884,#6881,#4489,.T.);
#8308=EDGE_CURVE('',#6883,#6885,#4490,.T.);
#8309=EDGE_CURVE('',#6885,#6886,#4491,.T.);
#8310=EDGE_CURVE('',#6886,#6884,#4492,.T.);
#8311=EDGE_CURVE('',#6885,#6887,#4493,.T.);
#8312=EDGE_CURVE('',#6887,#6888,#4494,.T.);
#8313=EDGE_CURVE('',#6888,#6886,#4495,.T.);
#8314=EDGE_CURVE('',#6887,#6889,#4496,.T.);
#8315=EDGE_CURVE('',#6889,#6890,#4497,.T.);
#8316=EDGE_CURVE('',#6890,#6888,#4498,.T.);
#8317=EDGE_CURVE('',#6889,#6879,#4499,.T.);
#8318=EDGE_CURVE('',#6882,#6890,#4500,.T.);
#8319=EDGE_CURVE('',#6891,#6891,#5926,.T.);
#8320=EDGE_CURVE('',#6892,#6892,#5927,.T.);
#8321=EDGE_CURVE('',#6893,#6893,#5928,.T.);
#8322=EDGE_CURVE('',#6893,#6892,#4501,.T.);
#8323=EDGE_CURVE('',#6894,#6894,#5929,.T.);
#8324=EDGE_CURVE('',#6894,#6893,#4502,.T.);
#8325=EDGE_CURVE('',#6895,#6895,#5930,.T.);
#8326=EDGE_CURVE('',#6895,#6894,#4503,.T.);
#8327=EDGE_CURVE('',#6896,#6896,#5931,.T.);
#8328=EDGE_CURVE('',#6897,#6897,#5932,.F.);
#8329=EDGE_CURVE('',#6897,#6896,#4504,.T.);
#8330=EDGE_CURVE('',#6891,#6897,#4505,.T.);
#8331=EDGE_CURVE('',#6898,#6898,#5933,.T.);
#8332=EDGE_CURVE('',#6898,#6899,#4506,.T.);
#8333=EDGE_CURVE('',#6899,#6899,#5934,.T.);
#8334=EDGE_CURVE('',#6900,#6901,#4507,.T.);
#8335=EDGE_CURVE('',#6902,#6900,#5935,.T.);
#8336=EDGE_CURVE('',#6903,#6902,#4508,.T.);
#8337=EDGE_CURVE('',#6903,#6901,#5936,.T.);
#8338=EDGE_CURVE('',#6904,#6903,#4509,.T.);
#8339=EDGE_CURVE('',#6905,#6904,#5937,.T.);
#8340=EDGE_CURVE('',#6901,#6905,#4510,.T.);
#8341=EDGE_CURVE('',#6906,#6906,#5938,.T.);
#8342=EDGE_CURVE('',#6907,#6902,#4511,.T.);
#8343=EDGE_CURVE('',#6907,#6904,#4512,.T.);
#8344=EDGE_CURVE('',#6906,#6908,#4513,.T.);
#8345=EDGE_CURVE('',#6908,#6908,#5939,.T.);
#8346=EDGE_CURVE('',#6905,#6909,#4514,.T.);
#8347=EDGE_CURVE('',#6909,#6907,#5940,.T.);
#8348=EDGE_CURVE('',#6900,#6909,#4515,.T.);
#8349=EDGE_CURVE('',#6910,#6910,#5941,.T.);
#8350=EDGE_CURVE('',#6910,#6911,#4516,.T.);
#8351=EDGE_CURVE('',#6911,#6911,#5942,.T.);
#8352=EDGE_CURVE('',#6912,#6912,#5943,.T.);
#8353=EDGE_CURVE('',#6912,#6913,#4517,.T.);
#8354=EDGE_CURVE('',#6913,#6913,#5944,.T.);
#8355=EDGE_CURVE('',#6914,#6914,#5945,.T.);
#8356=EDGE_CURVE('',#6914,#6915,#4518,.T.);
#8357=EDGE_CURVE('',#6915,#6915,#5946,.T.);
#8358=EDGE_CURVE('',#6916,#6916,#5947,.T.);
#8359=EDGE_CURVE('',#6916,#6917,#4519,.T.);
#8360=EDGE_CURVE('',#6917,#6917,#5948,.T.);
#8361=EDGE_CURVE('',#6918,#6918,#5949,.T.);
#8362=EDGE_CURVE('',#6918,#6919,#4520,.T.);
#8363=EDGE_CURVE('',#6919,#6919,#5950,.T.);
#8364=EDGE_CURVE('',#6920,#6920,#5951,.T.);
#8365=EDGE_CURVE('',#6920,#6921,#4521,.T.);
#8366=EDGE_CURVE('',#6921,#6921,#5952,.T.);
#8367=EDGE_CURVE('',#6922,#6922,#5953,.T.);
#8368=EDGE_CURVE('',#6922,#6923,#4522,.T.);
#8369=EDGE_CURVE('',#6923,#6923,#5954,.T.);
#8370=EDGE_CURVE('',#6924,#6924,#5955,.T.);
#8371=EDGE_CURVE('',#6924,#6925,#4523,.T.);
#8372=EDGE_CURVE('',#6925,#6925,#5956,.T.);
#8373=ORIENTED_EDGE('',*,*,#6926,.F.);
#8374=ORIENTED_EDGE('',*,*,#6927,.T.);
#8375=ORIENTED_EDGE('',*,*,#6928,.F.);
#8376=ORIENTED_EDGE('',*,*,#6927,.F.);
#8377=ORIENTED_EDGE('',*,*,#6929,.F.);
#8378=ORIENTED_EDGE('',*,*,#6930,.T.);
#8379=ORIENTED_EDGE('',*,*,#6931,.F.);
#8380=ORIENTED_EDGE('',*,*,#6930,.F.);
#8381=ORIENTED_EDGE('',*,*,#6932,.F.);
#8382=ORIENTED_EDGE('',*,*,#6933,.T.);
#8383=ORIENTED_EDGE('',*,*,#6934,.F.);
#8384=ORIENTED_EDGE('',*,*,#6933,.F.);
#8385=ORIENTED_EDGE('',*,*,#6935,.F.);
#8386=ORIENTED_EDGE('',*,*,#6936,.T.);
#8387=ORIENTED_EDGE('',*,*,#6937,.F.);
#8388=ORIENTED_EDGE('',*,*,#6936,.F.);
#8389=ORIENTED_EDGE('',*,*,#6938,.F.);
#8390=ORIENTED_EDGE('',*,*,#6939,.T.);
#8391=ORIENTED_EDGE('',*,*,#6940,.F.);
#8392=ORIENTED_EDGE('',*,*,#6939,.F.);
#8393=ORIENTED_EDGE('',*,*,#6941,.F.);
#8394=ORIENTED_EDGE('',*,*,#6942,.T.);
#8395=ORIENTED_EDGE('',*,*,#6943,.F.);
#8396=ORIENTED_EDGE('',*,*,#6942,.F.);
#8397=ORIENTED_EDGE('',*,*,#6944,.F.);
#8398=ORIENTED_EDGE('',*,*,#6945,.T.);
#8399=ORIENTED_EDGE('',*,*,#6946,.F.);
#8400=ORIENTED_EDGE('',*,*,#6945,.F.);
#8401=ORIENTED_EDGE('',*,*,#6947,.F.);
#8402=ORIENTED_EDGE('',*,*,#6948,.T.);
#8403=ORIENTED_EDGE('',*,*,#6949,.F.);
#8404=ORIENTED_EDGE('',*,*,#6948,.F.);
#8405=ORIENTED_EDGE('',*,*,#6950,.F.);
#8406=ORIENTED_EDGE('',*,*,#6951,.T.);
#8407=ORIENTED_EDGE('',*,*,#6952,.F.);
#8408=ORIENTED_EDGE('',*,*,#6951,.F.);
#8409=ORIENTED_EDGE('',*,*,#6953,.F.);
#8410=ORIENTED_EDGE('',*,*,#6954,.T.);
#8411=ORIENTED_EDGE('',*,*,#6955,.F.);
#8412=ORIENTED_EDGE('',*,*,#6954,.F.);
#8413=ORIENTED_EDGE('',*,*,#6956,.F.);
#8414=ORIENTED_EDGE('',*,*,#6957,.T.);
#8415=ORIENTED_EDGE('',*,*,#6958,.F.);
#8416=ORIENTED_EDGE('',*,*,#6957,.F.);
#8417=ORIENTED_EDGE('',*,*,#6959,.F.);
#8418=ORIENTED_EDGE('',*,*,#6960,.T.);
#8419=ORIENTED_EDGE('',*,*,#6961,.F.);
#8420=ORIENTED_EDGE('',*,*,#6960,.F.);
#8421=ORIENTED_EDGE('',*,*,#6962,.T.);
#8422=ORIENTED_EDGE('',*,*,#6963,.T.);
#8423=ORIENTED_EDGE('',*,*,#6964,.F.);
#8424=ORIENTED_EDGE('',*,*,#6965,.F.);
#8425=ORIENTED_EDGE('',*,*,#6966,.T.);
#8426=ORIENTED_EDGE('',*,*,#6965,.T.);
#8427=ORIENTED_EDGE('',*,*,#6967,.F.);
#8428=ORIENTED_EDGE('',*,*,#6968,.F.);
#8429=ORIENTED_EDGE('',*,*,#6969,.T.);
#8430=ORIENTED_EDGE('',*,*,#6968,.T.);
#8431=ORIENTED_EDGE('',*,*,#6970,.F.);
#8432=ORIENTED_EDGE('',*,*,#6971,.F.);
#8433=ORIENTED_EDGE('',*,*,#6972,.T.);
#8434=ORIENTED_EDGE('',*,*,#6971,.T.);
#8435=ORIENTED_EDGE('',*,*,#6973,.F.);
#8436=ORIENTED_EDGE('',*,*,#6963,.F.);
#8437=ORIENTED_EDGE('',*,*,#6973,.T.);
#8438=ORIENTED_EDGE('',*,*,#6970,.T.);
#8439=ORIENTED_EDGE('',*,*,#6967,.T.);
#8440=ORIENTED_EDGE('',*,*,#6964,.T.);
#8441=ORIENTED_EDGE('',*,*,#6931,.T.);
#8442=ORIENTED_EDGE('',*,*,#6937,.T.);
#8443=ORIENTED_EDGE('',*,*,#6961,.T.);
#8444=ORIENTED_EDGE('',*,*,#6958,.T.);
#8445=ORIENTED_EDGE('',*,*,#6955,.T.);
#8446=ORIENTED_EDGE('',*,*,#6952,.T.);
#8447=ORIENTED_EDGE('',*,*,#6949,.T.);
#8448=ORIENTED_EDGE('',*,*,#6946,.T.);
#8449=ORIENTED_EDGE('',*,*,#6943,.T.);
#8450=ORIENTED_EDGE('',*,*,#6940,.T.);
#8451=ORIENTED_EDGE('',*,*,#6934,.T.);
#8452=ORIENTED_EDGE('',*,*,#6928,.T.);
#8453=ORIENTED_EDGE('',*,*,#6972,.F.);
#8454=ORIENTED_EDGE('',*,*,#6962,.F.);
#8455=ORIENTED_EDGE('',*,*,#6966,.F.);
#8456=ORIENTED_EDGE('',*,*,#6969,.F.);
#8457=ORIENTED_EDGE('',*,*,#6929,.T.);
#8458=ORIENTED_EDGE('',*,*,#6935,.T.);
#8459=ORIENTED_EDGE('',*,*,#6959,.T.);
#8460=ORIENTED_EDGE('',*,*,#6956,.T.);
#8461=ORIENTED_EDGE('',*,*,#6953,.T.);
#8462=ORIENTED_EDGE('',*,*,#6950,.T.);
#8463=ORIENTED_EDGE('',*,*,#6947,.T.);
#8464=ORIENTED_EDGE('',*,*,#6944,.T.);
#8465=ORIENTED_EDGE('',*,*,#6941,.T.);
#8466=ORIENTED_EDGE('',*,*,#6938,.T.);
#8467=ORIENTED_EDGE('',*,*,#6932,.T.);
#8468=ORIENTED_EDGE('',*,*,#6926,.T.);
#8469=ORIENTED_EDGE('',*,*,#6974,.T.);
#8470=ORIENTED_EDGE('',*,*,#6975,.T.);
#8471=ORIENTED_EDGE('',*,*,#6976,.F.);
#8472=ORIENTED_EDGE('',*,*,#6977,.F.);
#8473=ORIENTED_EDGE('',*,*,#6978,.T.);
#8474=ORIENTED_EDGE('',*,*,#6977,.T.);
#8475=ORIENTED_EDGE('',*,*,#6979,.F.);
#8476=ORIENTED_EDGE('',*,*,#6980,.F.);
#8477=ORIENTED_EDGE('',*,*,#6981,.T.);
#8478=ORIENTED_EDGE('',*,*,#6980,.T.);
#8479=ORIENTED_EDGE('',*,*,#6982,.F.);
#8480=ORIENTED_EDGE('',*,*,#6983,.F.);
#8481=ORIENTED_EDGE('',*,*,#6984,.T.);
#8482=ORIENTED_EDGE('',*,*,#6983,.T.);
#8483=ORIENTED_EDGE('',*,*,#6985,.F.);
#8484=ORIENTED_EDGE('',*,*,#6975,.F.);
#8485=ORIENTED_EDGE('',*,*,#6985,.T.);
#8486=ORIENTED_EDGE('',*,*,#6982,.T.);
#8487=ORIENTED_EDGE('',*,*,#6979,.T.);
#8488=ORIENTED_EDGE('',*,*,#6976,.T.);
#8489=ORIENTED_EDGE('',*,*,#6984,.F.);
#8490=ORIENTED_EDGE('',*,*,#6974,.F.);
#8491=ORIENTED_EDGE('',*,*,#6978,.F.);
#8492=ORIENTED_EDGE('',*,*,#6981,.F.);
#8493=ORIENTED_EDGE('',*,*,#6986,.T.);
#8494=ORIENTED_EDGE('',*,*,#6987,.T.);
#8495=ORIENTED_EDGE('',*,*,#6988,.F.);
#8496=ORIENTED_EDGE('',*,*,#6989,.F.);
#8497=ORIENTED_EDGE('',*,*,#6990,.T.);
#8498=ORIENTED_EDGE('',*,*,#6989,.T.);
#8499=ORIENTED_EDGE('',*,*,#6991,.F.);
#8500=ORIENTED_EDGE('',*,*,#6992,.F.);
#8501=ORIENTED_EDGE('',*,*,#6993,.T.);
#8502=ORIENTED_EDGE('',*,*,#6992,.T.);
#8503=ORIENTED_EDGE('',*,*,#6994,.F.);
#8504=ORIENTED_EDGE('',*,*,#6995,.F.);
#8505=ORIENTED_EDGE('',*,*,#6996,.T.);
#8506=ORIENTED_EDGE('',*,*,#6995,.T.);
#8507=ORIENTED_EDGE('',*,*,#6997,.F.);
#8508=ORIENTED_EDGE('',*,*,#6987,.F.);
#8509=ORIENTED_EDGE('',*,*,#6997,.T.);
#8510=ORIENTED_EDGE('',*,*,#6994,.T.);
#8511=ORIENTED_EDGE('',*,*,#6991,.T.);
#8512=ORIENTED_EDGE('',*,*,#6988,.T.);
#8513=ORIENTED_EDGE('',*,*,#6996,.F.);
#8514=ORIENTED_EDGE('',*,*,#6986,.F.);
#8515=ORIENTED_EDGE('',*,*,#6990,.F.);
#8516=ORIENTED_EDGE('',*,*,#6993,.F.);
#8517=ORIENTED_EDGE('',*,*,#6998,.F.);
#8518=ORIENTED_EDGE('',*,*,#6999,.T.);
#8519=ORIENTED_EDGE('',*,*,#7000,.F.);
#8520=ORIENTED_EDGE('',*,*,#6999,.F.);
#8521=ORIENTED_EDGE('',*,*,#7001,.F.);
#8522=ORIENTED_EDGE('',*,*,#7002,.T.);
#8523=ORIENTED_EDGE('',*,*,#7003,.F.);
#8524=ORIENTED_EDGE('',*,*,#7002,.F.);
#8525=ORIENTED_EDGE('',*,*,#7004,.F.);
#8526=ORIENTED_EDGE('',*,*,#7005,.T.);
#8527=ORIENTED_EDGE('',*,*,#7006,.F.);
#8528=ORIENTED_EDGE('',*,*,#7005,.F.);
#8529=ORIENTED_EDGE('',*,*,#7007,.F.);
#8530=ORIENTED_EDGE('',*,*,#7008,.T.);
#8531=ORIENTED_EDGE('',*,*,#7009,.F.);
#8532=ORIENTED_EDGE('',*,*,#7008,.F.);
#8533=ORIENTED_EDGE('',*,*,#7010,.F.);
#8534=ORIENTED_EDGE('',*,*,#7011,.T.);
#8535=ORIENTED_EDGE('',*,*,#7012,.F.);
#8536=ORIENTED_EDGE('',*,*,#7011,.F.);
#8537=ORIENTED_EDGE('',*,*,#7013,.F.);
#8538=ORIENTED_EDGE('',*,*,#7014,.T.);
#8539=ORIENTED_EDGE('',*,*,#7015,.F.);
#8540=ORIENTED_EDGE('',*,*,#7014,.F.);
#8541=ORIENTED_EDGE('',*,*,#7016,.F.);
#8542=ORIENTED_EDGE('',*,*,#7017,.T.);
#8543=ORIENTED_EDGE('',*,*,#7018,.F.);
#8544=ORIENTED_EDGE('',*,*,#7017,.F.);
#8545=ORIENTED_EDGE('',*,*,#7019,.F.);
#8546=ORIENTED_EDGE('',*,*,#7020,.T.);
#8547=ORIENTED_EDGE('',*,*,#7021,.F.);
#8548=ORIENTED_EDGE('',*,*,#7020,.F.);
#8549=ORIENTED_EDGE('',*,*,#7022,.F.);
#8550=ORIENTED_EDGE('',*,*,#7023,.F.);
#8551=ORIENTED_EDGE('',*,*,#7024,.F.);
#8552=ORIENTED_EDGE('',*,*,#7025,.F.);
#8553=ORIENTED_EDGE('',*,*,#7026,.T.);
#8554=ORIENTED_EDGE('',*,*,#7027,.F.);
#8555=ORIENTED_EDGE('',*,*,#7028,.F.);
#8556=ORIENTED_EDGE('',*,*,#7029,.F.);
#8557=ORIENTED_EDGE('',*,*,#7012,.T.);
#8558=ORIENTED_EDGE('',*,*,#7015,.T.);
#8559=ORIENTED_EDGE('',*,*,#7018,.T.);
#8560=ORIENTED_EDGE('',*,*,#7021,.T.);
#8561=ORIENTED_EDGE('',*,*,#7030,.F.);
#8562=ORIENTED_EDGE('',*,*,#7028,.T.);
#8563=ORIENTED_EDGE('',*,*,#7031,.F.);
#8564=ORIENTED_EDGE('',*,*,#7032,.F.);
#8565=ORIENTED_EDGE('',*,*,#7033,.F.);
#8566=ORIENTED_EDGE('',*,*,#7034,.T.);
#8567=ORIENTED_EDGE('',*,*,#7035,.F.);
#8568=ORIENTED_EDGE('',*,*,#7026,.F.);
#8569=ORIENTED_EDGE('',*,*,#7027,.T.);
#8570=ORIENTED_EDGE('',*,*,#7035,.T.);
#8571=ORIENTED_EDGE('',*,*,#7036,.T.);
#8572=ORIENTED_EDGE('',*,*,#7031,.T.);
#8573=ORIENTED_EDGE('',*,*,#7037,.T.);
#8574=ORIENTED_EDGE('',*,*,#7038,.F.);
#8575=ORIENTED_EDGE('',*,*,#7039,.F.);
#8576=ORIENTED_EDGE('',*,*,#7029,.T.);
#8577=ORIENTED_EDGE('',*,*,#7030,.T.);
#8578=ORIENTED_EDGE('',*,*,#7040,.T.);
#8579=ORIENTED_EDGE('',*,*,#7033,.T.);
#8580=ORIENTED_EDGE('',*,*,#7025,.T.);
#8581=ORIENTED_EDGE('',*,*,#6998,.T.);
#8582=ORIENTED_EDGE('',*,*,#7001,.T.);
#8583=ORIENTED_EDGE('',*,*,#7004,.T.);
#8584=ORIENTED_EDGE('',*,*,#7007,.T.);
#8585=ORIENTED_EDGE('',*,*,#7024,.T.);
#8586=ORIENTED_EDGE('',*,*,#7041,.T.);
#8587=ORIENTED_EDGE('',*,*,#7042,.F.);
#8588=ORIENTED_EDGE('',*,*,#7037,.F.);
#8589=ORIENTED_EDGE('',*,*,#7023,.T.);
#8590=ORIENTED_EDGE('',*,*,#7043,.T.);
#8591=ORIENTED_EDGE('',*,*,#7044,.F.);
#8592=ORIENTED_EDGE('',*,*,#7041,.F.);
#8593=ORIENTED_EDGE('',*,*,#7000,.T.);
#8594=ORIENTED_EDGE('',*,*,#7003,.T.);
#8595=ORIENTED_EDGE('',*,*,#7006,.T.);
#8596=ORIENTED_EDGE('',*,*,#7009,.T.);
#8597=ORIENTED_EDGE('',*,*,#7022,.T.);
#8598=ORIENTED_EDGE('',*,*,#7039,.T.);
#8599=ORIENTED_EDGE('',*,*,#7045,.F.);
#8600=ORIENTED_EDGE('',*,*,#7043,.F.);
#8601=ORIENTED_EDGE('',*,*,#7045,.T.);
#8602=ORIENTED_EDGE('',*,*,#7038,.T.);
#8603=ORIENTED_EDGE('',*,*,#7042,.T.);
#8604=ORIENTED_EDGE('',*,*,#7044,.T.);
#8605=ORIENTED_EDGE('',*,*,#7040,.F.);
#8606=ORIENTED_EDGE('',*,*,#7032,.T.);
#8607=ORIENTED_EDGE('',*,*,#7036,.F.);
#8608=ORIENTED_EDGE('',*,*,#7034,.F.);
#8609=ORIENTED_EDGE('',*,*,#7010,.T.);
#8610=ORIENTED_EDGE('',*,*,#7013,.T.);
#8611=ORIENTED_EDGE('',*,*,#7016,.T.);
#8612=ORIENTED_EDGE('',*,*,#7019,.T.);
#8613=ORIENTED_EDGE('',*,*,#7046,.F.);
#8614=ORIENTED_EDGE('',*,*,#7047,.T.);
#8615=ORIENTED_EDGE('',*,*,#7048,.F.);
#8616=ORIENTED_EDGE('',*,*,#7047,.F.);
#8617=ORIENTED_EDGE('',*,*,#7049,.F.);
#8618=ORIENTED_EDGE('',*,*,#7050,.T.);
#8619=ORIENTED_EDGE('',*,*,#7051,.F.);
#8620=ORIENTED_EDGE('',*,*,#7050,.F.);
#8621=ORIENTED_EDGE('',*,*,#7052,.F.);
#8622=ORIENTED_EDGE('',*,*,#7053,.T.);
#8623=ORIENTED_EDGE('',*,*,#7054,.F.);
#8624=ORIENTED_EDGE('',*,*,#7053,.F.);
#8625=ORIENTED_EDGE('',*,*,#7055,.F.);
#8626=ORIENTED_EDGE('',*,*,#7056,.T.);
#8627=ORIENTED_EDGE('',*,*,#7057,.F.);
#8628=ORIENTED_EDGE('',*,*,#7056,.F.);
#8629=ORIENTED_EDGE('',*,*,#7058,.F.);
#8630=ORIENTED_EDGE('',*,*,#7059,.T.);
#8631=ORIENTED_EDGE('',*,*,#7060,.F.);
#8632=ORIENTED_EDGE('',*,*,#7059,.F.);
#8633=ORIENTED_EDGE('',*,*,#7061,.F.);
#8634=ORIENTED_EDGE('',*,*,#7062,.T.);
#8635=ORIENTED_EDGE('',*,*,#7063,.F.);
#8636=ORIENTED_EDGE('',*,*,#7062,.F.);
#8637=ORIENTED_EDGE('',*,*,#7064,.F.);
#8638=ORIENTED_EDGE('',*,*,#7065,.T.);
#8639=ORIENTED_EDGE('',*,*,#7066,.F.);
#8640=ORIENTED_EDGE('',*,*,#7065,.F.);
#8641=ORIENTED_EDGE('',*,*,#7067,.F.);
#8642=ORIENTED_EDGE('',*,*,#7068,.T.);
#8643=ORIENTED_EDGE('',*,*,#7069,.F.);
#8644=ORIENTED_EDGE('',*,*,#7068,.F.);
#8645=ORIENTED_EDGE('',*,*,#7070,.F.);
#8646=ORIENTED_EDGE('',*,*,#7071,.F.);
#8647=ORIENTED_EDGE('',*,*,#7072,.F.);
#8648=ORIENTED_EDGE('',*,*,#7073,.F.);
#8649=ORIENTED_EDGE('',*,*,#7074,.T.);
#8650=ORIENTED_EDGE('',*,*,#7075,.F.);
#8651=ORIENTED_EDGE('',*,*,#7076,.F.);
#8652=ORIENTED_EDGE('',*,*,#7077,.F.);
#8653=ORIENTED_EDGE('',*,*,#7060,.T.);
#8654=ORIENTED_EDGE('',*,*,#7063,.T.);
#8655=ORIENTED_EDGE('',*,*,#7066,.T.);
#8656=ORIENTED_EDGE('',*,*,#7069,.T.);
#8657=ORIENTED_EDGE('',*,*,#7078,.F.);
#8658=ORIENTED_EDGE('',*,*,#7076,.T.);
#8659=ORIENTED_EDGE('',*,*,#7079,.F.);
#8660=ORIENTED_EDGE('',*,*,#7080,.F.);
#8661=ORIENTED_EDGE('',*,*,#7081,.F.);
#8662=ORIENTED_EDGE('',*,*,#7082,.T.);
#8663=ORIENTED_EDGE('',*,*,#7083,.F.);
#8664=ORIENTED_EDGE('',*,*,#7074,.F.);
#8665=ORIENTED_EDGE('',*,*,#7075,.T.);
#8666=ORIENTED_EDGE('',*,*,#7083,.T.);
#8667=ORIENTED_EDGE('',*,*,#7084,.T.);
#8668=ORIENTED_EDGE('',*,*,#7079,.T.);
#8669=ORIENTED_EDGE('',*,*,#7085,.T.);
#8670=ORIENTED_EDGE('',*,*,#7086,.F.);
#8671=ORIENTED_EDGE('',*,*,#7087,.F.);
#8672=ORIENTED_EDGE('',*,*,#7077,.T.);
#8673=ORIENTED_EDGE('',*,*,#7078,.T.);
#8674=ORIENTED_EDGE('',*,*,#7088,.T.);
#8675=ORIENTED_EDGE('',*,*,#7081,.T.);
#8676=ORIENTED_EDGE('',*,*,#7073,.T.);
#8677=ORIENTED_EDGE('',*,*,#7046,.T.);
#8678=ORIENTED_EDGE('',*,*,#7049,.T.);
#8679=ORIENTED_EDGE('',*,*,#7052,.T.);
#8680=ORIENTED_EDGE('',*,*,#7055,.T.);
#8681=ORIENTED_EDGE('',*,*,#7072,.T.);
#8682=ORIENTED_EDGE('',*,*,#7089,.T.);
#8683=ORIENTED_EDGE('',*,*,#7090,.F.);
#8684=ORIENTED_EDGE('',*,*,#7085,.F.);
#8685=ORIENTED_EDGE('',*,*,#7071,.T.);
#8686=ORIENTED_EDGE('',*,*,#7091,.T.);
#8687=ORIENTED_EDGE('',*,*,#7092,.F.);
#8688=ORIENTED_EDGE('',*,*,#7089,.F.);
#8689=ORIENTED_EDGE('',*,*,#7048,.T.);
#8690=ORIENTED_EDGE('',*,*,#7051,.T.);
#8691=ORIENTED_EDGE('',*,*,#7054,.T.);
#8692=ORIENTED_EDGE('',*,*,#7057,.T.);
#8693=ORIENTED_EDGE('',*,*,#7070,.T.);
#8694=ORIENTED_EDGE('',*,*,#7087,.T.);
#8695=ORIENTED_EDGE('',*,*,#7093,.F.);
#8696=ORIENTED_EDGE('',*,*,#7091,.F.);
#8697=ORIENTED_EDGE('',*,*,#7093,.T.);
#8698=ORIENTED_EDGE('',*,*,#7086,.T.);
#8699=ORIENTED_EDGE('',*,*,#7090,.T.);
#8700=ORIENTED_EDGE('',*,*,#7092,.T.);
#8701=ORIENTED_EDGE('',*,*,#7088,.F.);
#8702=ORIENTED_EDGE('',*,*,#7080,.T.);
#8703=ORIENTED_EDGE('',*,*,#7084,.F.);
#8704=ORIENTED_EDGE('',*,*,#7082,.F.);
#8705=ORIENTED_EDGE('',*,*,#7058,.T.);
#8706=ORIENTED_EDGE('',*,*,#7061,.T.);
#8707=ORIENTED_EDGE('',*,*,#7064,.T.);
#8708=ORIENTED_EDGE('',*,*,#7067,.T.);
#8709=ORIENTED_EDGE('',*,*,#7094,.F.);
#8710=ORIENTED_EDGE('',*,*,#7095,.T.);
#8711=ORIENTED_EDGE('',*,*,#7096,.T.);
#8712=ORIENTED_EDGE('',*,*,#7095,.F.);
#8713=ORIENTED_EDGE('',*,*,#7096,.F.);
#8714=ORIENTED_EDGE('',*,*,#7097,.F.);
#8715=ORIENTED_EDGE('',*,*,#7098,.T.);
#8716=ORIENTED_EDGE('',*,*,#7099,.F.);
#8717=ORIENTED_EDGE('',*,*,#7098,.F.);
#8718=ORIENTED_EDGE('',*,*,#7100,.F.);
#8719=ORIENTED_EDGE('',*,*,#7101,.T.);
#8720=ORIENTED_EDGE('',*,*,#7102,.F.);
#8721=ORIENTED_EDGE('',*,*,#7101,.F.);
#8722=ORIENTED_EDGE('',*,*,#7103,.F.);
#8723=ORIENTED_EDGE('',*,*,#7104,.T.);
#8724=ORIENTED_EDGE('',*,*,#7105,.F.);
#8725=ORIENTED_EDGE('',*,*,#7104,.F.);
#8726=ORIENTED_EDGE('',*,*,#7106,.T.);
#8727=ORIENTED_EDGE('',*,*,#7099,.T.);
#8728=ORIENTED_EDGE('',*,*,#7102,.T.);
#8729=ORIENTED_EDGE('',*,*,#7105,.T.);
#8730=ORIENTED_EDGE('',*,*,#7107,.F.);
#8731=ORIENTED_EDGE('',*,*,#7108,.F.);
#8732=ORIENTED_EDGE('',*,*,#7097,.T.);
#8733=ORIENTED_EDGE('',*,*,#7100,.T.);
#8734=ORIENTED_EDGE('',*,*,#7103,.T.);
#8735=ORIENTED_EDGE('',*,*,#7109,.F.);
#8736=ORIENTED_EDGE('',*,*,#7106,.F.);
#8737=ORIENTED_EDGE('',*,*,#7110,.T.);
#8738=ORIENTED_EDGE('',*,*,#7108,.T.);
#8739=ORIENTED_EDGE('',*,*,#7110,.F.);
#8740=ORIENTED_EDGE('',*,*,#7109,.T.);
#8741=ORIENTED_EDGE('',*,*,#7111,.T.);
#8742=ORIENTED_EDGE('',*,*,#7112,.T.);
#8743=ORIENTED_EDGE('',*,*,#7111,.F.);
#8744=ORIENTED_EDGE('',*,*,#7113,.F.);
#8745=ORIENTED_EDGE('',*,*,#7114,.T.);
#8746=ORIENTED_EDGE('',*,*,#7107,.T.);
#8747=ORIENTED_EDGE('',*,*,#7114,.F.);
#8748=ORIENTED_EDGE('',*,*,#7113,.T.);
#8749=ORIENTED_EDGE('',*,*,#7112,.F.);
#8750=ORIENTED_EDGE('',*,*,#7094,.T.);
#8751=ORIENTED_EDGE('',*,*,#7115,.F.);
#8752=ORIENTED_EDGE('',*,*,#7116,.T.);
#8753=ORIENTED_EDGE('',*,*,#7117,.T.);
#8754=ORIENTED_EDGE('',*,*,#7116,.F.);
#8755=ORIENTED_EDGE('',*,*,#7118,.F.);
#8756=ORIENTED_EDGE('',*,*,#7119,.T.);
#8757=ORIENTED_EDGE('',*,*,#7120,.T.);
#8758=ORIENTED_EDGE('',*,*,#7119,.F.);
#8759=ORIENTED_EDGE('',*,*,#7118,.T.);
#8760=ORIENTED_EDGE('',*,*,#7115,.T.);
#8761=ORIENTED_EDGE('',*,*,#7120,.F.);
#8762=ORIENTED_EDGE('',*,*,#7117,.F.);
#8763=ORIENTED_EDGE('',*,*,#7121,.F.);
#8764=ORIENTED_EDGE('',*,*,#7122,.T.);
#8765=ORIENTED_EDGE('',*,*,#7123,.T.);
#8766=ORIENTED_EDGE('',*,*,#7122,.F.);
#8767=ORIENTED_EDGE('',*,*,#7124,.F.);
#8768=ORIENTED_EDGE('',*,*,#7125,.T.);
#8769=ORIENTED_EDGE('',*,*,#7126,.T.);
#8770=ORIENTED_EDGE('',*,*,#7125,.F.);
#8771=ORIENTED_EDGE('',*,*,#7124,.T.);
#8772=ORIENTED_EDGE('',*,*,#7121,.T.);
#8773=ORIENTED_EDGE('',*,*,#7126,.F.);
#8774=ORIENTED_EDGE('',*,*,#7123,.F.);
#8775=ORIENTED_EDGE('',*,*,#7127,.F.);
#8776=ORIENTED_EDGE('',*,*,#7128,.T.);
#8777=ORIENTED_EDGE('',*,*,#7129,.T.);
#8778=ORIENTED_EDGE('',*,*,#7128,.F.);
#8779=ORIENTED_EDGE('',*,*,#7130,.F.);
#8780=ORIENTED_EDGE('',*,*,#7131,.T.);
#8781=ORIENTED_EDGE('',*,*,#7132,.T.);
#8782=ORIENTED_EDGE('',*,*,#7131,.F.);
#8783=ORIENTED_EDGE('',*,*,#7130,.T.);
#8784=ORIENTED_EDGE('',*,*,#7127,.T.);
#8785=ORIENTED_EDGE('',*,*,#7132,.F.);
#8786=ORIENTED_EDGE('',*,*,#7129,.F.);
#8787=ORIENTED_EDGE('',*,*,#7133,.F.);
#8788=ORIENTED_EDGE('',*,*,#7134,.T.);
#8789=ORIENTED_EDGE('',*,*,#7135,.T.);
#8790=ORIENTED_EDGE('',*,*,#7134,.F.);
#8791=ORIENTED_EDGE('',*,*,#7135,.F.);
#8792=ORIENTED_EDGE('',*,*,#7136,.F.);
#8793=ORIENTED_EDGE('',*,*,#7137,.T.);
#8794=ORIENTED_EDGE('',*,*,#7138,.F.);
#8795=ORIENTED_EDGE('',*,*,#7137,.F.);
#8796=ORIENTED_EDGE('',*,*,#7139,.F.);
#8797=ORIENTED_EDGE('',*,*,#7140,.T.);
#8798=ORIENTED_EDGE('',*,*,#7141,.F.);
#8799=ORIENTED_EDGE('',*,*,#7140,.F.);
#8800=ORIENTED_EDGE('',*,*,#7142,.F.);
#8801=ORIENTED_EDGE('',*,*,#7143,.T.);
#8802=ORIENTED_EDGE('',*,*,#7144,.F.);
#8803=ORIENTED_EDGE('',*,*,#7143,.F.);
#8804=ORIENTED_EDGE('',*,*,#7145,.T.);
#8805=ORIENTED_EDGE('',*,*,#7138,.T.);
#8806=ORIENTED_EDGE('',*,*,#7141,.T.);
#8807=ORIENTED_EDGE('',*,*,#7144,.T.);
#8808=ORIENTED_EDGE('',*,*,#7146,.F.);
#8809=ORIENTED_EDGE('',*,*,#7147,.F.);
#8810=ORIENTED_EDGE('',*,*,#7136,.T.);
#8811=ORIENTED_EDGE('',*,*,#7139,.T.);
#8812=ORIENTED_EDGE('',*,*,#7142,.T.);
#8813=ORIENTED_EDGE('',*,*,#7148,.F.);
#8814=ORIENTED_EDGE('',*,*,#7145,.F.);
#8815=ORIENTED_EDGE('',*,*,#7149,.T.);
#8816=ORIENTED_EDGE('',*,*,#7147,.T.);
#8817=ORIENTED_EDGE('',*,*,#7149,.F.);
#8818=ORIENTED_EDGE('',*,*,#7148,.T.);
#8819=ORIENTED_EDGE('',*,*,#7150,.T.);
#8820=ORIENTED_EDGE('',*,*,#7151,.T.);
#8821=ORIENTED_EDGE('',*,*,#7150,.F.);
#8822=ORIENTED_EDGE('',*,*,#7152,.F.);
#8823=ORIENTED_EDGE('',*,*,#7153,.T.);
#8824=ORIENTED_EDGE('',*,*,#7146,.T.);
#8825=ORIENTED_EDGE('',*,*,#7153,.F.);
#8826=ORIENTED_EDGE('',*,*,#7152,.T.);
#8827=ORIENTED_EDGE('',*,*,#7151,.F.);
#8828=ORIENTED_EDGE('',*,*,#7133,.T.);
#8829=ORIENTED_EDGE('',*,*,#7154,.F.);
#8830=ORIENTED_EDGE('',*,*,#7155,.T.);
#8831=ORIENTED_EDGE('',*,*,#7156,.T.);
#8832=ORIENTED_EDGE('',*,*,#7155,.F.);
#8833=ORIENTED_EDGE('',*,*,#7157,.F.);
#8834=ORIENTED_EDGE('',*,*,#7158,.T.);
#8835=ORIENTED_EDGE('',*,*,#7159,.T.);
#8836=ORIENTED_EDGE('',*,*,#7158,.F.);
#8837=ORIENTED_EDGE('',*,*,#7157,.T.);
#8838=ORIENTED_EDGE('',*,*,#7154,.T.);
#8839=ORIENTED_EDGE('',*,*,#7159,.F.);
#8840=ORIENTED_EDGE('',*,*,#7156,.F.);
#8841=ORIENTED_EDGE('',*,*,#7160,.F.);
#8842=ORIENTED_EDGE('',*,*,#7161,.T.);
#8843=ORIENTED_EDGE('',*,*,#7162,.T.);
#8844=ORIENTED_EDGE('',*,*,#7161,.F.);
#8845=ORIENTED_EDGE('',*,*,#7163,.F.);
#8846=ORIENTED_EDGE('',*,*,#7164,.T.);
#8847=ORIENTED_EDGE('',*,*,#7165,.T.);
#8848=ORIENTED_EDGE('',*,*,#7164,.F.);
#8849=ORIENTED_EDGE('',*,*,#7163,.T.);
#8850=ORIENTED_EDGE('',*,*,#7160,.T.);
#8851=ORIENTED_EDGE('',*,*,#7165,.F.);
#8852=ORIENTED_EDGE('',*,*,#7162,.F.);
#8853=ORIENTED_EDGE('',*,*,#7166,.F.);
#8854=ORIENTED_EDGE('',*,*,#7167,.T.);
#8855=ORIENTED_EDGE('',*,*,#7168,.T.);
#8856=ORIENTED_EDGE('',*,*,#7167,.F.);
#8857=ORIENTED_EDGE('',*,*,#7169,.F.);
#8858=ORIENTED_EDGE('',*,*,#7170,.T.);
#8859=ORIENTED_EDGE('',*,*,#7171,.T.);
#8860=ORIENTED_EDGE('',*,*,#7170,.F.);
#8861=ORIENTED_EDGE('',*,*,#7169,.T.);
#8862=ORIENTED_EDGE('',*,*,#7166,.T.);
#8863=ORIENTED_EDGE('',*,*,#7171,.F.);
#8864=ORIENTED_EDGE('',*,*,#7168,.F.);
#8865=ORIENTED_EDGE('',*,*,#7172,.F.);
#8866=ORIENTED_EDGE('',*,*,#7173,.F.);
#8867=ORIENTED_EDGE('',*,*,#7174,.F.);
#8868=ORIENTED_EDGE('',*,*,#7175,.F.);
#8869=ORIENTED_EDGE('',*,*,#7176,.F.);
#8870=ORIENTED_EDGE('',*,*,#7177,.T.);
#8871=ORIENTED_EDGE('',*,*,#7178,.F.);
#8872=ORIENTED_EDGE('',*,*,#7177,.F.);
#8873=ORIENTED_EDGE('',*,*,#7173,.T.);
#8874=ORIENTED_EDGE('',*,*,#7179,.T.);
#8875=ORIENTED_EDGE('',*,*,#7180,.T.);
#8876=ORIENTED_EDGE('',*,*,#7181,.T.);
#8877=ORIENTED_EDGE('',*,*,#7182,.T.);
#8878=ORIENTED_EDGE('',*,*,#7174,.T.);
#8879=ORIENTED_EDGE('',*,*,#7181,.F.);
#8880=ORIENTED_EDGE('',*,*,#7183,.F.);
#8881=ORIENTED_EDGE('',*,*,#7184,.T.);
#8882=ORIENTED_EDGE('',*,*,#7185,.T.);
#8883=ORIENTED_EDGE('',*,*,#7186,.F.);
#8884=ORIENTED_EDGE('',*,*,#7187,.T.);
#8885=ORIENTED_EDGE('',*,*,#7188,.T.);
#8886=ORIENTED_EDGE('',*,*,#7189,.T.);
#8887=ORIENTED_EDGE('',*,*,#7178,.T.);
#8888=ORIENTED_EDGE('',*,*,#7190,.F.);
#8889=ORIENTED_EDGE('',*,*,#7191,.T.);
#8890=ORIENTED_EDGE('',*,*,#7192,.F.);
#8891=ORIENTED_EDGE('',*,*,#7191,.F.);
#8892=ORIENTED_EDGE('',*,*,#7190,.T.);
#8893=ORIENTED_EDGE('',*,*,#7193,.F.);
#8894=ORIENTED_EDGE('',*,*,#7194,.F.);
#8895=ORIENTED_EDGE('',*,*,#7195,.T.);
#8896=ORIENTED_EDGE('',*,*,#7193,.T.);
#8897=ORIENTED_EDGE('',*,*,#7195,.F.);
#8898=ORIENTED_EDGE('',*,*,#7196,.F.);
#8899=ORIENTED_EDGE('',*,*,#7197,.T.);
#8900=ORIENTED_EDGE('',*,*,#7182,.F.);
#8901=ORIENTED_EDGE('',*,*,#7197,.F.);
#8902=ORIENTED_EDGE('',*,*,#7196,.T.);
#8903=ORIENTED_EDGE('',*,*,#7198,.F.);
#8904=ORIENTED_EDGE('',*,*,#7199,.F.);
#8905=ORIENTED_EDGE('',*,*,#7200,.T.);
#8906=ORIENTED_EDGE('',*,*,#7198,.T.);
#8907=ORIENTED_EDGE('',*,*,#7200,.F.);
#8908=ORIENTED_EDGE('',*,*,#7201,.F.);
#8909=ORIENTED_EDGE('',*,*,#7202,.T.);
#8910=ORIENTED_EDGE('',*,*,#7189,.F.);
#8911=ORIENTED_EDGE('',*,*,#7202,.F.);
#8912=ORIENTED_EDGE('',*,*,#7203,.F.);
#8913=ORIENTED_EDGE('',*,*,#7204,.T.);
#8914=ORIENTED_EDGE('',*,*,#7188,.F.);
#8915=ORIENTED_EDGE('',*,*,#7204,.F.);
#8916=ORIENTED_EDGE('',*,*,#7205,.F.);
#8917=ORIENTED_EDGE('',*,*,#7206,.T.);
#8918=ORIENTED_EDGE('',*,*,#7187,.F.);
#8919=ORIENTED_EDGE('',*,*,#7206,.F.);
#8920=ORIENTED_EDGE('',*,*,#7207,.T.);
#8921=ORIENTED_EDGE('',*,*,#7208,.T.);
#8922=ORIENTED_EDGE('',*,*,#7209,.F.);
#8923=ORIENTED_EDGE('',*,*,#7185,.F.);
#8924=ORIENTED_EDGE('',*,*,#7210,.T.);
#8925=ORIENTED_EDGE('',*,*,#7183,.T.);
#8926=ORIENTED_EDGE('',*,*,#7180,.F.);
#8927=ORIENTED_EDGE('',*,*,#7211,.F.);
#8928=ORIENTED_EDGE('',*,*,#7172,.T.);
#8929=ORIENTED_EDGE('',*,*,#7212,.F.);
#8930=ORIENTED_EDGE('',*,*,#7208,.F.);
#8931=ORIENTED_EDGE('',*,*,#7213,.T.);
#8932=ORIENTED_EDGE('',*,*,#7211,.T.);
#8933=ORIENTED_EDGE('',*,*,#7179,.F.);
#8934=ORIENTED_EDGE('',*,*,#7176,.T.);
#8935=ORIENTED_EDGE('',*,*,#7201,.T.);
#8936=ORIENTED_EDGE('',*,*,#7203,.T.);
#8937=ORIENTED_EDGE('',*,*,#7205,.T.);
#8938=ORIENTED_EDGE('',*,*,#7175,.T.);
#8939=ORIENTED_EDGE('',*,*,#7186,.T.);
#8940=ORIENTED_EDGE('',*,*,#7209,.T.);
#8941=ORIENTED_EDGE('',*,*,#7212,.T.);
#8942=ORIENTED_EDGE('',*,*,#7192,.T.);
#8943=ORIENTED_EDGE('',*,*,#7213,.F.);
#8944=ORIENTED_EDGE('',*,*,#7207,.F.);
#8945=ORIENTED_EDGE('',*,*,#7184,.F.);
#8946=ORIENTED_EDGE('',*,*,#7210,.F.);
#8947=ORIENTED_EDGE('',*,*,#7194,.T.);
#8948=ORIENTED_EDGE('',*,*,#7199,.T.);
#8949=ORIENTED_EDGE('',*,*,#7214,.F.);
#8950=ORIENTED_EDGE('',*,*,#7215,.T.);
#8951=ORIENTED_EDGE('',*,*,#7216,.F.);
#8952=ORIENTED_EDGE('',*,*,#7215,.F.);
#8953=ORIENTED_EDGE('',*,*,#7217,.F.);
#8954=ORIENTED_EDGE('',*,*,#7218,.T.);
#8955=ORIENTED_EDGE('',*,*,#7219,.F.);
#8956=ORIENTED_EDGE('',*,*,#7218,.F.);
#8957=ORIENTED_EDGE('',*,*,#7220,.F.);
#8958=ORIENTED_EDGE('',*,*,#7221,.F.);
#8959=ORIENTED_EDGE('',*,*,#7222,.F.);
#8960=ORIENTED_EDGE('',*,*,#7223,.F.);
#8961=ORIENTED_EDGE('',*,*,#7224,.F.);
#8962=ORIENTED_EDGE('',*,*,#7225,.F.);
#8963=ORIENTED_EDGE('',*,*,#7226,.F.);
#8964=ORIENTED_EDGE('',*,*,#7227,.F.);
#8965=ORIENTED_EDGE('',*,*,#7221,.T.);
#8966=ORIENTED_EDGE('',*,*,#7228,.T.);
#8967=ORIENTED_EDGE('',*,*,#7225,.T.);
#8968=ORIENTED_EDGE('',*,*,#7229,.T.);
#8969=ORIENTED_EDGE('',*,*,#7216,.T.);
#8970=ORIENTED_EDGE('',*,*,#7219,.T.);
#8971=ORIENTED_EDGE('',*,*,#7230,.T.);
#8972=ORIENTED_EDGE('',*,*,#7220,.T.);
#8973=ORIENTED_EDGE('',*,*,#7231,.T.);
#8974=ORIENTED_EDGE('',*,*,#7226,.T.);
#8975=ORIENTED_EDGE('',*,*,#7228,.F.);
#8976=ORIENTED_EDGE('',*,*,#7222,.T.);
#8977=ORIENTED_EDGE('',*,*,#7229,.F.);
#8978=ORIENTED_EDGE('',*,*,#7224,.T.);
#8979=ORIENTED_EDGE('',*,*,#7232,.T.);
#8980=ORIENTED_EDGE('',*,*,#7230,.F.);
#8981=ORIENTED_EDGE('',*,*,#7233,.T.);
#8982=ORIENTED_EDGE('',*,*,#7234,.T.);
#8983=ORIENTED_EDGE('',*,*,#7233,.F.);
#8984=ORIENTED_EDGE('',*,*,#7223,.T.);
#8985=ORIENTED_EDGE('',*,*,#7232,.F.);
#8986=ORIENTED_EDGE('',*,*,#7227,.T.);
#8987=ORIENTED_EDGE('',*,*,#7231,.F.);
#8988=ORIENTED_EDGE('',*,*,#7214,.T.);
#8989=ORIENTED_EDGE('',*,*,#7217,.T.);
#8990=ORIENTED_EDGE('',*,*,#7234,.F.);
#8991=ORIENTED_EDGE('',*,*,#7235,.T.);
#8992=ORIENTED_EDGE('',*,*,#7236,.F.);
#8993=ORIENTED_EDGE('',*,*,#7235,.F.);
#8994=ORIENTED_EDGE('',*,*,#7237,.T.);
#8995=ORIENTED_EDGE('',*,*,#7238,.T.);
#8996=ORIENTED_EDGE('',*,*,#7237,.F.);
#8997=ORIENTED_EDGE('',*,*,#7238,.F.);
#8998=ORIENTED_EDGE('',*,*,#7239,.F.);
#8999=ORIENTED_EDGE('',*,*,#7240,.T.);
#9000=ORIENTED_EDGE('',*,*,#7236,.T.);
#9001=ORIENTED_EDGE('',*,*,#7240,.F.);
#9002=ORIENTED_EDGE('',*,*,#7239,.T.);
#9003=ORIENTED_EDGE('',*,*,#7241,.T.);
#9004=ORIENTED_EDGE('',*,*,#7242,.F.);
#9005=ORIENTED_EDGE('',*,*,#7241,.F.);
#9006=ORIENTED_EDGE('',*,*,#7243,.T.);
#9007=ORIENTED_EDGE('',*,*,#7244,.T.);
#9008=ORIENTED_EDGE('',*,*,#7243,.F.);
#9009=ORIENTED_EDGE('',*,*,#7244,.F.);
#9010=ORIENTED_EDGE('',*,*,#7245,.F.);
#9011=ORIENTED_EDGE('',*,*,#7246,.T.);
#9012=ORIENTED_EDGE('',*,*,#7242,.T.);
#9013=ORIENTED_EDGE('',*,*,#7246,.F.);
#9014=ORIENTED_EDGE('',*,*,#7245,.T.);
#9015=ORIENTED_EDGE('',*,*,#7247,.F.);
#9016=ORIENTED_EDGE('',*,*,#7248,.T.);
#9017=ORIENTED_EDGE('',*,*,#7249,.F.);
#9018=ORIENTED_EDGE('',*,*,#7248,.F.);
#9019=ORIENTED_EDGE('',*,*,#7250,.F.);
#9020=ORIENTED_EDGE('',*,*,#7251,.T.);
#9021=ORIENTED_EDGE('',*,*,#7252,.F.);
#9022=ORIENTED_EDGE('',*,*,#7251,.F.);
#9023=ORIENTED_EDGE('',*,*,#7253,.F.);
#9024=ORIENTED_EDGE('',*,*,#7254,.F.);
#9025=ORIENTED_EDGE('',*,*,#7255,.F.);
#9026=ORIENTED_EDGE('',*,*,#7256,.F.);
#9027=ORIENTED_EDGE('',*,*,#7257,.F.);
#9028=ORIENTED_EDGE('',*,*,#7258,.F.);
#9029=ORIENTED_EDGE('',*,*,#7259,.F.);
#9030=ORIENTED_EDGE('',*,*,#7260,.F.);
#9031=ORIENTED_EDGE('',*,*,#7254,.T.);
#9032=ORIENTED_EDGE('',*,*,#7261,.T.);
#9033=ORIENTED_EDGE('',*,*,#7258,.T.);
#9034=ORIENTED_EDGE('',*,*,#7262,.T.);
#9035=ORIENTED_EDGE('',*,*,#7249,.T.);
#9036=ORIENTED_EDGE('',*,*,#7252,.T.);
#9037=ORIENTED_EDGE('',*,*,#7263,.T.);
#9038=ORIENTED_EDGE('',*,*,#7253,.T.);
#9039=ORIENTED_EDGE('',*,*,#7264,.T.);
#9040=ORIENTED_EDGE('',*,*,#7259,.T.);
#9041=ORIENTED_EDGE('',*,*,#7261,.F.);
#9042=ORIENTED_EDGE('',*,*,#7255,.T.);
#9043=ORIENTED_EDGE('',*,*,#7262,.F.);
#9044=ORIENTED_EDGE('',*,*,#7257,.T.);
#9045=ORIENTED_EDGE('',*,*,#7265,.T.);
#9046=ORIENTED_EDGE('',*,*,#7263,.F.);
#9047=ORIENTED_EDGE('',*,*,#7266,.T.);
#9048=ORIENTED_EDGE('',*,*,#7267,.T.);
#9049=ORIENTED_EDGE('',*,*,#7266,.F.);
#9050=ORIENTED_EDGE('',*,*,#7256,.T.);
#9051=ORIENTED_EDGE('',*,*,#7265,.F.);
#9052=ORIENTED_EDGE('',*,*,#7260,.T.);
#9053=ORIENTED_EDGE('',*,*,#7264,.F.);
#9054=ORIENTED_EDGE('',*,*,#7247,.T.);
#9055=ORIENTED_EDGE('',*,*,#7250,.T.);
#9056=ORIENTED_EDGE('',*,*,#7267,.F.);
#9057=ORIENTED_EDGE('',*,*,#7268,.F.);
#9058=ORIENTED_EDGE('',*,*,#7269,.T.);
#9059=ORIENTED_EDGE('',*,*,#7270,.F.);
#9060=ORIENTED_EDGE('',*,*,#7271,.T.);
#9061=ORIENTED_EDGE('',*,*,#7268,.T.);
#9062=ORIENTED_EDGE('',*,*,#7271,.F.);
#9063=ORIENTED_EDGE('',*,*,#7270,.T.);
#9064=ORIENTED_EDGE('',*,*,#7269,.F.);
#9065=ORIENTED_EDGE('',*,*,#7272,.T.);
#9066=ORIENTED_EDGE('',*,*,#7273,.T.);
#9067=ORIENTED_EDGE('',*,*,#7272,.F.);
#9068=ORIENTED_EDGE('',*,*,#7273,.F.);
#9069=ORIENTED_EDGE('',*,*,#7274,.F.);
#9070=ORIENTED_EDGE('',*,*,#7275,.T.);
#9071=ORIENTED_EDGE('',*,*,#7276,.F.);
#9072=ORIENTED_EDGE('',*,*,#7277,.T.);
#9073=ORIENTED_EDGE('',*,*,#7274,.T.);
#9074=ORIENTED_EDGE('',*,*,#7277,.F.);
#9075=ORIENTED_EDGE('',*,*,#7276,.T.);
#9076=ORIENTED_EDGE('',*,*,#7275,.F.);
#9077=ORIENTED_EDGE('',*,*,#7278,.T.);
#9078=ORIENTED_EDGE('',*,*,#7279,.T.);
#9079=ORIENTED_EDGE('',*,*,#7278,.F.);
#9080=ORIENTED_EDGE('',*,*,#7279,.F.);
#9081=ORIENTED_EDGE('',*,*,#7280,.F.);
#9082=ORIENTED_EDGE('',*,*,#7281,.F.);
#9083=ORIENTED_EDGE('',*,*,#7282,.F.);
#9084=ORIENTED_EDGE('',*,*,#7283,.F.);
#9085=ORIENTED_EDGE('',*,*,#7284,.F.);
#9086=ORIENTED_EDGE('',*,*,#7285,.T.);
#9087=ORIENTED_EDGE('',*,*,#7286,.F.);
#9088=ORIENTED_EDGE('',*,*,#7285,.F.);
#9089=ORIENTED_EDGE('',*,*,#7281,.T.);
#9090=ORIENTED_EDGE('',*,*,#7287,.T.);
#9091=ORIENTED_EDGE('',*,*,#7288,.T.);
#9092=ORIENTED_EDGE('',*,*,#7289,.T.);
#9093=ORIENTED_EDGE('',*,*,#7290,.T.);
#9094=ORIENTED_EDGE('',*,*,#7282,.T.);
#9095=ORIENTED_EDGE('',*,*,#7289,.F.);
#9096=ORIENTED_EDGE('',*,*,#7291,.F.);
#9097=ORIENTED_EDGE('',*,*,#7292,.T.);
#9098=ORIENTED_EDGE('',*,*,#7293,.T.);
#9099=ORIENTED_EDGE('',*,*,#7294,.F.);
#9100=ORIENTED_EDGE('',*,*,#7295,.T.);
#9101=ORIENTED_EDGE('',*,*,#7296,.T.);
#9102=ORIENTED_EDGE('',*,*,#7297,.T.);
#9103=ORIENTED_EDGE('',*,*,#7286,.T.);
#9104=ORIENTED_EDGE('',*,*,#7298,.F.);
#9105=ORIENTED_EDGE('',*,*,#7299,.T.);
#9106=ORIENTED_EDGE('',*,*,#7300,.F.);
#9107=ORIENTED_EDGE('',*,*,#7299,.F.);
#9108=ORIENTED_EDGE('',*,*,#7298,.T.);
#9109=ORIENTED_EDGE('',*,*,#7301,.F.);
#9110=ORIENTED_EDGE('',*,*,#7302,.F.);
#9111=ORIENTED_EDGE('',*,*,#7303,.T.);
#9112=ORIENTED_EDGE('',*,*,#7301,.T.);
#9113=ORIENTED_EDGE('',*,*,#7303,.F.);
#9114=ORIENTED_EDGE('',*,*,#7304,.F.);
#9115=ORIENTED_EDGE('',*,*,#7305,.T.);
#9116=ORIENTED_EDGE('',*,*,#7290,.F.);
#9117=ORIENTED_EDGE('',*,*,#7305,.F.);
#9118=ORIENTED_EDGE('',*,*,#7304,.T.);
#9119=ORIENTED_EDGE('',*,*,#7306,.F.);
#9120=ORIENTED_EDGE('',*,*,#7307,.F.);
#9121=ORIENTED_EDGE('',*,*,#7308,.T.);
#9122=ORIENTED_EDGE('',*,*,#7306,.T.);
#9123=ORIENTED_EDGE('',*,*,#7308,.F.);
#9124=ORIENTED_EDGE('',*,*,#7309,.F.);
#9125=ORIENTED_EDGE('',*,*,#7310,.T.);
#9126=ORIENTED_EDGE('',*,*,#7297,.F.);
#9127=ORIENTED_EDGE('',*,*,#7310,.F.);
#9128=ORIENTED_EDGE('',*,*,#7311,.F.);
#9129=ORIENTED_EDGE('',*,*,#7312,.T.);
#9130=ORIENTED_EDGE('',*,*,#7296,.F.);
#9131=ORIENTED_EDGE('',*,*,#7312,.F.);
#9132=ORIENTED_EDGE('',*,*,#7313,.F.);
#9133=ORIENTED_EDGE('',*,*,#7314,.T.);
#9134=ORIENTED_EDGE('',*,*,#7295,.F.);
#9135=ORIENTED_EDGE('',*,*,#7314,.F.);
#9136=ORIENTED_EDGE('',*,*,#7315,.T.);
#9137=ORIENTED_EDGE('',*,*,#7316,.T.);
#9138=ORIENTED_EDGE('',*,*,#7317,.F.);
#9139=ORIENTED_EDGE('',*,*,#7293,.F.);
#9140=ORIENTED_EDGE('',*,*,#7318,.T.);
#9141=ORIENTED_EDGE('',*,*,#7291,.T.);
#9142=ORIENTED_EDGE('',*,*,#7288,.F.);
#9143=ORIENTED_EDGE('',*,*,#7319,.F.);
#9144=ORIENTED_EDGE('',*,*,#7280,.T.);
#9145=ORIENTED_EDGE('',*,*,#7320,.F.);
#9146=ORIENTED_EDGE('',*,*,#7316,.F.);
#9147=ORIENTED_EDGE('',*,*,#7321,.T.);
#9148=ORIENTED_EDGE('',*,*,#7319,.T.);
#9149=ORIENTED_EDGE('',*,*,#7287,.F.);
#9150=ORIENTED_EDGE('',*,*,#7284,.T.);
#9151=ORIENTED_EDGE('',*,*,#7309,.T.);
#9152=ORIENTED_EDGE('',*,*,#7311,.T.);
#9153=ORIENTED_EDGE('',*,*,#7313,.T.);
#9154=ORIENTED_EDGE('',*,*,#7283,.T.);
#9155=ORIENTED_EDGE('',*,*,#7294,.T.);
#9156=ORIENTED_EDGE('',*,*,#7317,.T.);
#9157=ORIENTED_EDGE('',*,*,#7320,.T.);
#9158=ORIENTED_EDGE('',*,*,#7300,.T.);
#9159=ORIENTED_EDGE('',*,*,#7321,.F.);
#9160=ORIENTED_EDGE('',*,*,#7315,.F.);
#9161=ORIENTED_EDGE('',*,*,#7292,.F.);
#9162=ORIENTED_EDGE('',*,*,#7318,.F.);
#9163=ORIENTED_EDGE('',*,*,#7302,.T.);
#9164=ORIENTED_EDGE('',*,*,#7307,.T.);
#9165=ORIENTED_EDGE('',*,*,#7322,.F.);
#9166=ORIENTED_EDGE('',*,*,#7323,.T.);
#9167=ORIENTED_EDGE('',*,*,#7324,.F.);
#9168=ORIENTED_EDGE('',*,*,#7323,.F.);
#9169=ORIENTED_EDGE('',*,*,#7325,.F.);
#9170=ORIENTED_EDGE('',*,*,#7326,.T.);
#9171=ORIENTED_EDGE('',*,*,#7327,.F.);
#9172=ORIENTED_EDGE('',*,*,#7326,.F.);
#9173=ORIENTED_EDGE('',*,*,#7328,.F.);
#9174=ORIENTED_EDGE('',*,*,#7329,.F.);
#9175=ORIENTED_EDGE('',*,*,#7330,.F.);
#9176=ORIENTED_EDGE('',*,*,#7331,.F.);
#9177=ORIENTED_EDGE('',*,*,#7332,.F.);
#9178=ORIENTED_EDGE('',*,*,#7333,.F.);
#9179=ORIENTED_EDGE('',*,*,#7334,.F.);
#9180=ORIENTED_EDGE('',*,*,#7335,.F.);
#9181=ORIENTED_EDGE('',*,*,#7329,.T.);
#9182=ORIENTED_EDGE('',*,*,#7336,.T.);
#9183=ORIENTED_EDGE('',*,*,#7333,.T.);
#9184=ORIENTED_EDGE('',*,*,#7337,.T.);
#9185=ORIENTED_EDGE('',*,*,#7324,.T.);
#9186=ORIENTED_EDGE('',*,*,#7327,.T.);
#9187=ORIENTED_EDGE('',*,*,#7338,.T.);
#9188=ORIENTED_EDGE('',*,*,#7328,.T.);
#9189=ORIENTED_EDGE('',*,*,#7339,.T.);
#9190=ORIENTED_EDGE('',*,*,#7334,.T.);
#9191=ORIENTED_EDGE('',*,*,#7336,.F.);
#9192=ORIENTED_EDGE('',*,*,#7330,.T.);
#9193=ORIENTED_EDGE('',*,*,#7337,.F.);
#9194=ORIENTED_EDGE('',*,*,#7332,.T.);
#9195=ORIENTED_EDGE('',*,*,#7340,.T.);
#9196=ORIENTED_EDGE('',*,*,#7338,.F.);
#9197=ORIENTED_EDGE('',*,*,#7341,.T.);
#9198=ORIENTED_EDGE('',*,*,#7342,.T.);
#9199=ORIENTED_EDGE('',*,*,#7341,.F.);
#9200=ORIENTED_EDGE('',*,*,#7331,.T.);
#9201=ORIENTED_EDGE('',*,*,#7340,.F.);
#9202=ORIENTED_EDGE('',*,*,#7335,.T.);
#9203=ORIENTED_EDGE('',*,*,#7339,.F.);
#9204=ORIENTED_EDGE('',*,*,#7322,.T.);
#9205=ORIENTED_EDGE('',*,*,#7325,.T.);
#9206=ORIENTED_EDGE('',*,*,#7342,.F.);
#9207=ORIENTED_EDGE('',*,*,#7343,.T.);
#9208=ORIENTED_EDGE('',*,*,#7344,.F.);
#9209=ORIENTED_EDGE('',*,*,#7343,.F.);
#9210=ORIENTED_EDGE('',*,*,#7345,.T.);
#9211=ORIENTED_EDGE('',*,*,#7346,.T.);
#9212=ORIENTED_EDGE('',*,*,#7345,.F.);
#9213=ORIENTED_EDGE('',*,*,#7346,.F.);
#9214=ORIENTED_EDGE('',*,*,#7347,.F.);
#9215=ORIENTED_EDGE('',*,*,#7348,.T.);
#9216=ORIENTED_EDGE('',*,*,#7344,.T.);
#9217=ORIENTED_EDGE('',*,*,#7348,.F.);
#9218=ORIENTED_EDGE('',*,*,#7347,.T.);
#9219=ORIENTED_EDGE('',*,*,#7349,.T.);
#9220=ORIENTED_EDGE('',*,*,#7350,.F.);
#9221=ORIENTED_EDGE('',*,*,#7349,.F.);
#9222=ORIENTED_EDGE('',*,*,#7351,.T.);
#9223=ORIENTED_EDGE('',*,*,#7352,.T.);
#9224=ORIENTED_EDGE('',*,*,#7351,.F.);
#9225=ORIENTED_EDGE('',*,*,#7352,.F.);
#9226=ORIENTED_EDGE('',*,*,#7353,.F.);
#9227=ORIENTED_EDGE('',*,*,#7354,.T.);
#9228=ORIENTED_EDGE('',*,*,#7350,.T.);
#9229=ORIENTED_EDGE('',*,*,#7354,.F.);
#9230=ORIENTED_EDGE('',*,*,#7353,.T.);
#9231=ORIENTED_EDGE('',*,*,#7355,.F.);
#9232=ORIENTED_EDGE('',*,*,#7356,.T.);
#9233=ORIENTED_EDGE('',*,*,#7357,.F.);
#9234=ORIENTED_EDGE('',*,*,#7356,.F.);
#9235=ORIENTED_EDGE('',*,*,#7358,.F.);
#9236=ORIENTED_EDGE('',*,*,#7359,.T.);
#9237=ORIENTED_EDGE('',*,*,#7360,.F.);
#9238=ORIENTED_EDGE('',*,*,#7359,.F.);
#9239=ORIENTED_EDGE('',*,*,#7361,.F.);
#9240=ORIENTED_EDGE('',*,*,#7362,.F.);
#9241=ORIENTED_EDGE('',*,*,#7363,.F.);
#9242=ORIENTED_EDGE('',*,*,#7364,.F.);
#9243=ORIENTED_EDGE('',*,*,#7365,.F.);
#9244=ORIENTED_EDGE('',*,*,#7366,.F.);
#9245=ORIENTED_EDGE('',*,*,#7367,.F.);
#9246=ORIENTED_EDGE('',*,*,#7368,.F.);
#9247=ORIENTED_EDGE('',*,*,#7362,.T.);
#9248=ORIENTED_EDGE('',*,*,#7369,.T.);
#9249=ORIENTED_EDGE('',*,*,#7366,.T.);
#9250=ORIENTED_EDGE('',*,*,#7370,.T.);
#9251=ORIENTED_EDGE('',*,*,#7357,.T.);
#9252=ORIENTED_EDGE('',*,*,#7360,.T.);
#9253=ORIENTED_EDGE('',*,*,#7371,.T.);
#9254=ORIENTED_EDGE('',*,*,#7361,.T.);
#9255=ORIENTED_EDGE('',*,*,#7372,.T.);
#9256=ORIENTED_EDGE('',*,*,#7367,.T.);
#9257=ORIENTED_EDGE('',*,*,#7369,.F.);
#9258=ORIENTED_EDGE('',*,*,#7363,.T.);
#9259=ORIENTED_EDGE('',*,*,#7370,.F.);
#9260=ORIENTED_EDGE('',*,*,#7365,.T.);
#9261=ORIENTED_EDGE('',*,*,#7373,.T.);
#9262=ORIENTED_EDGE('',*,*,#7371,.F.);
#9263=ORIENTED_EDGE('',*,*,#7374,.T.);
#9264=ORIENTED_EDGE('',*,*,#7375,.T.);
#9265=ORIENTED_EDGE('',*,*,#7374,.F.);
#9266=ORIENTED_EDGE('',*,*,#7364,.T.);
#9267=ORIENTED_EDGE('',*,*,#7373,.F.);
#9268=ORIENTED_EDGE('',*,*,#7368,.T.);
#9269=ORIENTED_EDGE('',*,*,#7372,.F.);
#9270=ORIENTED_EDGE('',*,*,#7355,.T.);
#9271=ORIENTED_EDGE('',*,*,#7358,.T.);
#9272=ORIENTED_EDGE('',*,*,#7375,.F.);
#9273=ORIENTED_EDGE('',*,*,#7376,.F.);
#9274=ORIENTED_EDGE('',*,*,#7377,.T.);
#9275=ORIENTED_EDGE('',*,*,#7378,.F.);
#9276=ORIENTED_EDGE('',*,*,#7379,.T.);
#9277=ORIENTED_EDGE('',*,*,#7376,.T.);
#9278=ORIENTED_EDGE('',*,*,#7379,.F.);
#9279=ORIENTED_EDGE('',*,*,#7378,.T.);
#9280=ORIENTED_EDGE('',*,*,#7377,.F.);
#9281=ORIENTED_EDGE('',*,*,#7380,.T.);
#9282=ORIENTED_EDGE('',*,*,#7381,.T.);
#9283=ORIENTED_EDGE('',*,*,#7380,.F.);
#9284=ORIENTED_EDGE('',*,*,#7381,.F.);
#9285=ORIENTED_EDGE('',*,*,#7382,.F.);
#9286=ORIENTED_EDGE('',*,*,#7383,.T.);
#9287=ORIENTED_EDGE('',*,*,#7384,.F.);
#9288=ORIENTED_EDGE('',*,*,#7385,.T.);
#9289=ORIENTED_EDGE('',*,*,#7382,.T.);
#9290=ORIENTED_EDGE('',*,*,#7385,.F.);
#9291=ORIENTED_EDGE('',*,*,#7384,.T.);
#9292=ORIENTED_EDGE('',*,*,#7383,.F.);
#9293=ORIENTED_EDGE('',*,*,#7386,.T.);
#9294=ORIENTED_EDGE('',*,*,#7387,.T.);
#9295=ORIENTED_EDGE('',*,*,#7386,.F.);
#9296=ORIENTED_EDGE('',*,*,#7387,.F.);
#9297=ORIENTED_EDGE('',*,*,#7388,.F.);
#9298=ORIENTED_EDGE('',*,*,#7389,.T.);
#9299=ORIENTED_EDGE('',*,*,#7390,.T.);
#9300=ORIENTED_EDGE('',*,*,#7389,.F.);
#9301=ORIENTED_EDGE('',*,*,#7388,.T.);
#9302=ORIENTED_EDGE('',*,*,#7390,.F.);
#9303=ORIENTED_EDGE('',*,*,#7391,.F.);
#9304=ORIENTED_EDGE('',*,*,#7392,.T.);
#9305=ORIENTED_EDGE('',*,*,#7393,.T.);
#9306=ORIENTED_EDGE('',*,*,#7392,.F.);
#9307=ORIENTED_EDGE('',*,*,#7391,.T.);
#9308=ORIENTED_EDGE('',*,*,#7393,.F.);
#9309=ORIENTED_EDGE('',*,*,#7394,.F.);
#9310=ORIENTED_EDGE('',*,*,#7395,.F.);
#9311=ORIENTED_EDGE('',*,*,#7396,.T.);
#9312=ORIENTED_EDGE('',*,*,#7394,.T.);
#9313=ORIENTED_EDGE('',*,*,#7396,.F.);
#9314=ORIENTED_EDGE('',*,*,#7397,.F.);
#9315=ORIENTED_EDGE('',*,*,#7398,.T.);
#9316=ORIENTED_EDGE('',*,*,#7395,.T.);
#9317=ORIENTED_EDGE('',*,*,#7398,.F.);
#9318=ORIENTED_EDGE('',*,*,#7399,.F.);
#9319=ORIENTED_EDGE('',*,*,#7400,.T.);
#9320=ORIENTED_EDGE('',*,*,#7397,.T.);
#9321=ORIENTED_EDGE('',*,*,#7400,.F.);
#9322=ORIENTED_EDGE('',*,*,#7399,.T.);
#9323=ORIENTED_EDGE('',*,*,#7401,.F.);
#9324=ORIENTED_EDGE('',*,*,#7402,.F.);
#9325=ORIENTED_EDGE('',*,*,#7403,.T.);
#9326=ORIENTED_EDGE('',*,*,#7401,.T.);
#9327=ORIENTED_EDGE('',*,*,#7403,.F.);
#9328=ORIENTED_EDGE('',*,*,#7404,.F.);
#9329=ORIENTED_EDGE('',*,*,#7405,.T.);
#9330=ORIENTED_EDGE('',*,*,#7402,.T.);
#9331=ORIENTED_EDGE('',*,*,#7405,.F.);
#9332=ORIENTED_EDGE('',*,*,#7406,.F.);
#9333=ORIENTED_EDGE('',*,*,#7407,.T.);
#9334=ORIENTED_EDGE('',*,*,#7404,.T.);
#9335=ORIENTED_EDGE('',*,*,#7407,.F.);
#9336=ORIENTED_EDGE('',*,*,#7406,.T.);
#9337=ORIENTED_EDGE('',*,*,#7408,.T.);
#9338=ORIENTED_EDGE('',*,*,#7409,.T.);
#9339=ORIENTED_EDGE('',*,*,#7410,.T.);
#9340=ORIENTED_EDGE('',*,*,#7411,.F.);
#9341=ORIENTED_EDGE('',*,*,#7412,.T.);
#9342=ORIENTED_EDGE('',*,*,#7413,.T.);
#9343=ORIENTED_EDGE('',*,*,#7414,.T.);
#9344=ORIENTED_EDGE('',*,*,#7409,.F.);
#9345=ORIENTED_EDGE('',*,*,#7415,.T.);
#9346=ORIENTED_EDGE('',*,*,#7416,.T.);
#9347=ORIENTED_EDGE('',*,*,#7417,.T.);
#9348=ORIENTED_EDGE('',*,*,#7413,.F.);
#9349=ORIENTED_EDGE('',*,*,#7418,.T.);
#9350=ORIENTED_EDGE('',*,*,#7419,.T.);
#9351=ORIENTED_EDGE('',*,*,#7420,.T.);
#9352=ORIENTED_EDGE('',*,*,#7416,.F.);
#9353=ORIENTED_EDGE('',*,*,#7421,.T.);
#9354=ORIENTED_EDGE('',*,*,#7422,.T.);
#9355=ORIENTED_EDGE('',*,*,#7423,.T.);
#9356=ORIENTED_EDGE('',*,*,#7419,.F.);
#9357=ORIENTED_EDGE('',*,*,#7424,.T.);
#9358=ORIENTED_EDGE('',*,*,#7411,.T.);
#9359=ORIENTED_EDGE('',*,*,#7425,.T.);
#9360=ORIENTED_EDGE('',*,*,#7422,.F.);
#9361=ORIENTED_EDGE('',*,*,#7424,.F.);
#9362=ORIENTED_EDGE('',*,*,#7421,.F.);
#9363=ORIENTED_EDGE('',*,*,#7418,.F.);
#9364=ORIENTED_EDGE('',*,*,#7415,.F.);
#9365=ORIENTED_EDGE('',*,*,#7412,.F.);
#9366=ORIENTED_EDGE('',*,*,#7408,.F.);
#9367=ORIENTED_EDGE('',*,*,#7425,.F.);
#9368=ORIENTED_EDGE('',*,*,#7410,.F.);
#9369=ORIENTED_EDGE('',*,*,#7414,.F.);
#9370=ORIENTED_EDGE('',*,*,#7417,.F.);
#9371=ORIENTED_EDGE('',*,*,#7420,.F.);
#9372=ORIENTED_EDGE('',*,*,#7423,.F.);
#9373=ORIENTED_EDGE('',*,*,#7426,.F.);
#9374=ORIENTED_EDGE('',*,*,#7427,.T.);
#9375=ORIENTED_EDGE('',*,*,#7428,.F.);
#9376=ORIENTED_EDGE('',*,*,#7427,.F.);
#9377=ORIENTED_EDGE('',*,*,#7429,.F.);
#9378=ORIENTED_EDGE('',*,*,#7430,.T.);
#9379=ORIENTED_EDGE('',*,*,#7431,.F.);
#9380=ORIENTED_EDGE('',*,*,#7430,.F.);
#9381=ORIENTED_EDGE('',*,*,#7432,.F.);
#9382=ORIENTED_EDGE('',*,*,#7433,.T.);
#9383=ORIENTED_EDGE('',*,*,#7434,.F.);
#9384=ORIENTED_EDGE('',*,*,#7433,.F.);
#9385=ORIENTED_EDGE('',*,*,#7435,.F.);
#9386=ORIENTED_EDGE('',*,*,#7436,.T.);
#9387=ORIENTED_EDGE('',*,*,#7437,.F.);
#9388=ORIENTED_EDGE('',*,*,#7436,.F.);
#9389=ORIENTED_EDGE('',*,*,#7438,.F.);
#9390=ORIENTED_EDGE('',*,*,#7439,.T.);
#9391=ORIENTED_EDGE('',*,*,#7440,.F.);
#9392=ORIENTED_EDGE('',*,*,#7439,.F.);
#9393=ORIENTED_EDGE('',*,*,#7441,.F.);
#9394=ORIENTED_EDGE('',*,*,#7442,.F.);
#9395=ORIENTED_EDGE('',*,*,#7443,.F.);
#9396=ORIENTED_EDGE('',*,*,#7444,.T.);
#9397=ORIENTED_EDGE('',*,*,#7444,.F.);
#9398=ORIENTED_EDGE('',*,*,#7445,.F.);
#9399=ORIENTED_EDGE('',*,*,#7446,.F.);
#9400=ORIENTED_EDGE('',*,*,#7447,.F.);
#9401=ORIENTED_EDGE('',*,*,#7448,.T.);
#9402=ORIENTED_EDGE('',*,*,#7449,.T.);
#9403=ORIENTED_EDGE('',*,*,#7450,.T.);
#9404=ORIENTED_EDGE('',*,*,#7451,.T.);
#9405=ORIENTED_EDGE('',*,*,#7452,.T.);
#9406=ORIENTED_EDGE('',*,*,#7438,.T.);
#9407=ORIENTED_EDGE('',*,*,#7435,.T.);
#9408=ORIENTED_EDGE('',*,*,#7432,.T.);
#9409=ORIENTED_EDGE('',*,*,#7429,.T.);
#9410=ORIENTED_EDGE('',*,*,#7426,.T.);
#9411=ORIENTED_EDGE('',*,*,#7443,.T.);
#9412=ORIENTED_EDGE('',*,*,#7453,.F.);
#9413=ORIENTED_EDGE('',*,*,#7454,.T.);
#9414=ORIENTED_EDGE('',*,*,#7445,.T.);
#9415=ORIENTED_EDGE('',*,*,#7452,.F.);
#9416=ORIENTED_EDGE('',*,*,#7455,.T.);
#9417=ORIENTED_EDGE('',*,*,#7456,.F.);
#9418=ORIENTED_EDGE('',*,*,#7455,.F.);
#9419=ORIENTED_EDGE('',*,*,#7451,.F.);
#9420=ORIENTED_EDGE('',*,*,#7457,.T.);
#9421=ORIENTED_EDGE('',*,*,#7458,.F.);
#9422=ORIENTED_EDGE('',*,*,#7457,.F.);
#9423=ORIENTED_EDGE('',*,*,#7450,.F.);
#9424=ORIENTED_EDGE('',*,*,#7459,.T.);
#9425=ORIENTED_EDGE('',*,*,#7460,.F.);
#9426=ORIENTED_EDGE('',*,*,#7459,.F.);
#9427=ORIENTED_EDGE('',*,*,#7449,.F.);
#9428=ORIENTED_EDGE('',*,*,#7461,.T.);
#9429=ORIENTED_EDGE('',*,*,#7462,.F.);
#9430=ORIENTED_EDGE('',*,*,#7461,.F.);
#9431=ORIENTED_EDGE('',*,*,#7448,.F.);
#9432=ORIENTED_EDGE('',*,*,#7463,.T.);
#9433=ORIENTED_EDGE('',*,*,#7464,.F.);
#9434=ORIENTED_EDGE('',*,*,#7463,.F.);
#9435=ORIENTED_EDGE('',*,*,#7465,.F.);
#9436=ORIENTED_EDGE('',*,*,#7446,.T.);
#9437=ORIENTED_EDGE('',*,*,#7454,.F.);
#9438=ORIENTED_EDGE('',*,*,#7466,.F.);
#9439=ORIENTED_EDGE('',*,*,#7441,.T.);
#9440=ORIENTED_EDGE('',*,*,#7447,.T.);
#9441=ORIENTED_EDGE('',*,*,#7465,.T.);
#9442=ORIENTED_EDGE('',*,*,#7467,.F.);
#9443=ORIENTED_EDGE('',*,*,#7467,.T.);
#9444=ORIENTED_EDGE('',*,*,#7466,.T.);
#9445=ORIENTED_EDGE('',*,*,#7453,.T.);
#9446=ORIENTED_EDGE('',*,*,#7442,.T.);
#9447=ORIENTED_EDGE('',*,*,#7456,.T.);
#9448=ORIENTED_EDGE('',*,*,#7458,.T.);
#9449=ORIENTED_EDGE('',*,*,#7460,.T.);
#9450=ORIENTED_EDGE('',*,*,#7462,.T.);
#9451=ORIENTED_EDGE('',*,*,#7464,.T.);
#9452=ORIENTED_EDGE('',*,*,#7440,.T.);
#9453=ORIENTED_EDGE('',*,*,#7437,.T.);
#9454=ORIENTED_EDGE('',*,*,#7434,.T.);
#9455=ORIENTED_EDGE('',*,*,#7431,.T.);
#9456=ORIENTED_EDGE('',*,*,#7428,.T.);
#9457=ORIENTED_EDGE('',*,*,#7468,.F.);
#9458=ORIENTED_EDGE('',*,*,#7469,.T.);
#9459=ORIENTED_EDGE('',*,*,#7470,.F.);
#9460=ORIENTED_EDGE('',*,*,#7469,.F.);
#9461=ORIENTED_EDGE('',*,*,#7471,.F.);
#9462=ORIENTED_EDGE('',*,*,#7472,.T.);
#9463=ORIENTED_EDGE('',*,*,#7473,.F.);
#9464=ORIENTED_EDGE('',*,*,#7472,.F.);
#9465=ORIENTED_EDGE('',*,*,#7474,.F.);
#9466=ORIENTED_EDGE('',*,*,#7475,.T.);
#9467=ORIENTED_EDGE('',*,*,#7476,.F.);
#9468=ORIENTED_EDGE('',*,*,#7475,.F.);
#9469=ORIENTED_EDGE('',*,*,#7477,.F.);
#9470=ORIENTED_EDGE('',*,*,#7478,.T.);
#9471=ORIENTED_EDGE('',*,*,#7479,.F.);
#9472=ORIENTED_EDGE('',*,*,#7478,.F.);
#9473=ORIENTED_EDGE('',*,*,#7480,.F.);
#9474=ORIENTED_EDGE('',*,*,#7481,.T.);
#9475=ORIENTED_EDGE('',*,*,#7482,.T.);
#9476=ORIENTED_EDGE('',*,*,#7481,.F.);
#9477=ORIENTED_EDGE('',*,*,#7483,.F.);
#9478=ORIENTED_EDGE('',*,*,#7484,.T.);
#9479=ORIENTED_EDGE('',*,*,#7485,.T.);
#9480=ORIENTED_EDGE('',*,*,#7484,.F.);
#9481=ORIENTED_EDGE('',*,*,#7483,.T.);
#9482=ORIENTED_EDGE('',*,*,#7480,.T.);
#9483=ORIENTED_EDGE('',*,*,#7479,.T.);
#9484=ORIENTED_EDGE('',*,*,#7476,.T.);
#9485=ORIENTED_EDGE('',*,*,#7473,.T.);
#9486=ORIENTED_EDGE('',*,*,#7470,.T.);
#9487=ORIENTED_EDGE('',*,*,#7485,.F.);
#9488=ORIENTED_EDGE('',*,*,#7482,.F.);
#9489=ORIENTED_EDGE('',*,*,#7477,.T.);
#9490=ORIENTED_EDGE('',*,*,#7474,.T.);
#9491=ORIENTED_EDGE('',*,*,#7471,.T.);
#9492=ORIENTED_EDGE('',*,*,#7468,.T.);
#9493=ORIENTED_EDGE('',*,*,#7486,.T.);
#9494=ORIENTED_EDGE('',*,*,#7487,.F.);
#9495=ORIENTED_EDGE('',*,*,#7486,.F.);
#9496=ORIENTED_EDGE('',*,*,#7488,.T.);
#9497=ORIENTED_EDGE('',*,*,#7489,.T.);
#9498=ORIENTED_EDGE('',*,*,#7488,.F.);
#9499=ORIENTED_EDGE('',*,*,#7489,.F.);
#9500=ORIENTED_EDGE('',*,*,#7490,.F.);
#9501=ORIENTED_EDGE('',*,*,#7491,.T.);
#9502=ORIENTED_EDGE('',*,*,#7487,.T.);
#9503=ORIENTED_EDGE('',*,*,#7491,.F.);
#9504=ORIENTED_EDGE('',*,*,#7490,.T.);
#9505=ORIENTED_EDGE('',*,*,#7492,.T.);
#9506=ORIENTED_EDGE('',*,*,#7493,.F.);
#9507=ORIENTED_EDGE('',*,*,#7492,.F.);
#9508=ORIENTED_EDGE('',*,*,#7494,.T.);
#9509=ORIENTED_EDGE('',*,*,#7495,.T.);
#9510=ORIENTED_EDGE('',*,*,#7494,.F.);
#9511=ORIENTED_EDGE('',*,*,#7495,.F.);
#9512=ORIENTED_EDGE('',*,*,#7496,.F.);
#9513=ORIENTED_EDGE('',*,*,#7497,.T.);
#9514=ORIENTED_EDGE('',*,*,#7493,.T.);
#9515=ORIENTED_EDGE('',*,*,#7497,.F.);
#9516=ORIENTED_EDGE('',*,*,#7496,.T.);
#9517=ORIENTED_EDGE('',*,*,#7498,.T.);
#9518=ORIENTED_EDGE('',*,*,#7499,.F.);
#9519=ORIENTED_EDGE('',*,*,#7498,.F.);
#9520=ORIENTED_EDGE('',*,*,#7500,.T.);
#9521=ORIENTED_EDGE('',*,*,#7501,.T.);
#9522=ORIENTED_EDGE('',*,*,#7500,.F.);
#9523=ORIENTED_EDGE('',*,*,#7501,.F.);
#9524=ORIENTED_EDGE('',*,*,#7502,.F.);
#9525=ORIENTED_EDGE('',*,*,#7503,.T.);
#9526=ORIENTED_EDGE('',*,*,#7499,.T.);
#9527=ORIENTED_EDGE('',*,*,#7503,.F.);
#9528=ORIENTED_EDGE('',*,*,#7502,.T.);
#9529=ORIENTED_EDGE('',*,*,#7504,.T.);
#9530=ORIENTED_EDGE('',*,*,#7505,.F.);
#9531=ORIENTED_EDGE('',*,*,#7504,.F.);
#9532=ORIENTED_EDGE('',*,*,#7506,.T.);
#9533=ORIENTED_EDGE('',*,*,#7507,.T.);
#9534=ORIENTED_EDGE('',*,*,#7506,.F.);
#9535=ORIENTED_EDGE('',*,*,#7507,.F.);
#9536=ORIENTED_EDGE('',*,*,#7508,.F.);
#9537=ORIENTED_EDGE('',*,*,#7509,.T.);
#9538=ORIENTED_EDGE('',*,*,#7505,.T.);
#9539=ORIENTED_EDGE('',*,*,#7509,.F.);
#9540=ORIENTED_EDGE('',*,*,#7508,.T.);
#9541=ORIENTED_EDGE('',*,*,#7510,.F.);
#9542=ORIENTED_EDGE('',*,*,#7511,.T.);
#9543=ORIENTED_EDGE('',*,*,#7512,.F.);
#9544=ORIENTED_EDGE('',*,*,#7511,.F.);
#9545=ORIENTED_EDGE('',*,*,#7513,.F.);
#9546=ORIENTED_EDGE('',*,*,#7514,.T.);
#9547=ORIENTED_EDGE('',*,*,#7515,.F.);
#9548=ORIENTED_EDGE('',*,*,#7514,.F.);
#9549=ORIENTED_EDGE('',*,*,#7516,.F.);
#9550=ORIENTED_EDGE('',*,*,#7517,.T.);
#9551=ORIENTED_EDGE('',*,*,#7518,.F.);
#9552=ORIENTED_EDGE('',*,*,#7517,.F.);
#9553=ORIENTED_EDGE('',*,*,#7519,.F.);
#9554=ORIENTED_EDGE('',*,*,#7520,.T.);
#9555=ORIENTED_EDGE('',*,*,#7521,.F.);
#9556=ORIENTED_EDGE('',*,*,#7520,.F.);
#9557=ORIENTED_EDGE('',*,*,#7522,.F.);
#9558=ORIENTED_EDGE('',*,*,#7523,.T.);
#9559=ORIENTED_EDGE('',*,*,#7524,.T.);
#9560=ORIENTED_EDGE('',*,*,#7523,.F.);
#9561=ORIENTED_EDGE('',*,*,#7525,.F.);
#9562=ORIENTED_EDGE('',*,*,#7526,.T.);
#9563=ORIENTED_EDGE('',*,*,#7527,.T.);
#9564=ORIENTED_EDGE('',*,*,#7526,.F.);
#9565=ORIENTED_EDGE('',*,*,#7525,.T.);
#9566=ORIENTED_EDGE('',*,*,#7522,.T.);
#9567=ORIENTED_EDGE('',*,*,#7521,.T.);
#9568=ORIENTED_EDGE('',*,*,#7518,.T.);
#9569=ORIENTED_EDGE('',*,*,#7515,.T.);
#9570=ORIENTED_EDGE('',*,*,#7512,.T.);
#9571=ORIENTED_EDGE('',*,*,#7527,.F.);
#9572=ORIENTED_EDGE('',*,*,#7524,.F.);
#9573=ORIENTED_EDGE('',*,*,#7519,.T.);
#9574=ORIENTED_EDGE('',*,*,#7516,.T.);
#9575=ORIENTED_EDGE('',*,*,#7513,.T.);
#9576=ORIENTED_EDGE('',*,*,#7510,.T.);
#9577=ORIENTED_EDGE('',*,*,#7528,.F.);
#9578=ORIENTED_EDGE('',*,*,#7529,.T.);
#9579=ORIENTED_EDGE('',*,*,#7530,.F.);
#9580=ORIENTED_EDGE('',*,*,#7531,.T.);
#9581=ORIENTED_EDGE('',*,*,#7528,.T.);
#9582=ORIENTED_EDGE('',*,*,#7531,.F.);
#9583=ORIENTED_EDGE('',*,*,#7530,.T.);
#9584=ORIENTED_EDGE('',*,*,#7529,.F.);
#9585=ORIENTED_EDGE('',*,*,#7532,.T.);
#9586=ORIENTED_EDGE('',*,*,#7533,.T.);
#9587=ORIENTED_EDGE('',*,*,#7532,.F.);
#9588=ORIENTED_EDGE('',*,*,#7533,.F.);
#9589=ORIENTED_EDGE('',*,*,#7534,.F.);
#9590=ORIENTED_EDGE('',*,*,#7535,.T.);
#9591=ORIENTED_EDGE('',*,*,#7536,.F.);
#9592=ORIENTED_EDGE('',*,*,#7537,.T.);
#9593=ORIENTED_EDGE('',*,*,#7534,.T.);
#9594=ORIENTED_EDGE('',*,*,#7537,.F.);
#9595=ORIENTED_EDGE('',*,*,#7536,.T.);
#9596=ORIENTED_EDGE('',*,*,#7535,.F.);
#9597=ORIENTED_EDGE('',*,*,#7538,.T.);
#9598=ORIENTED_EDGE('',*,*,#7539,.T.);
#9599=ORIENTED_EDGE('',*,*,#7538,.F.);
#9600=ORIENTED_EDGE('',*,*,#7539,.F.);
#9601=ORIENTED_EDGE('',*,*,#7540,.F.);
#9602=ORIENTED_EDGE('',*,*,#7541,.T.);
#9603=ORIENTED_EDGE('',*,*,#7542,.F.);
#9604=ORIENTED_EDGE('',*,*,#7543,.T.);
#9605=ORIENTED_EDGE('',*,*,#7540,.T.);
#9606=ORIENTED_EDGE('',*,*,#7543,.F.);
#9607=ORIENTED_EDGE('',*,*,#7542,.T.);
#9608=ORIENTED_EDGE('',*,*,#7541,.F.);
#9609=ORIENTED_EDGE('',*,*,#7544,.T.);
#9610=ORIENTED_EDGE('',*,*,#7545,.T.);
#9611=ORIENTED_EDGE('',*,*,#7544,.F.);
#9612=ORIENTED_EDGE('',*,*,#7545,.F.);
#9613=ORIENTED_EDGE('',*,*,#7546,.F.);
#9614=ORIENTED_EDGE('',*,*,#7547,.T.);
#9615=ORIENTED_EDGE('',*,*,#7548,.F.);
#9616=ORIENTED_EDGE('',*,*,#7549,.T.);
#9617=ORIENTED_EDGE('',*,*,#7546,.T.);
#9618=ORIENTED_EDGE('',*,*,#7549,.F.);
#9619=ORIENTED_EDGE('',*,*,#7548,.T.);
#9620=ORIENTED_EDGE('',*,*,#7547,.F.);
#9621=ORIENTED_EDGE('',*,*,#7550,.T.);
#9622=ORIENTED_EDGE('',*,*,#7551,.T.);
#9623=ORIENTED_EDGE('',*,*,#7550,.F.);
#9624=ORIENTED_EDGE('',*,*,#7551,.F.);
#9625=ORIENTED_EDGE('',*,*,#7552,.F.);
#9626=ORIENTED_EDGE('',*,*,#7553,.T.);
#9627=ORIENTED_EDGE('',*,*,#7554,.F.);
#9628=ORIENTED_EDGE('',*,*,#7553,.F.);
#9629=ORIENTED_EDGE('',*,*,#7555,.F.);
#9630=ORIENTED_EDGE('',*,*,#7556,.T.);
#9631=ORIENTED_EDGE('',*,*,#7557,.F.);
#9632=ORIENTED_EDGE('',*,*,#7556,.F.);
#9633=ORIENTED_EDGE('',*,*,#7558,.F.);
#9634=ORIENTED_EDGE('',*,*,#7559,.T.);
#9635=ORIENTED_EDGE('',*,*,#7560,.F.);
#9636=ORIENTED_EDGE('',*,*,#7559,.F.);
#9637=ORIENTED_EDGE('',*,*,#7561,.F.);
#9638=ORIENTED_EDGE('',*,*,#7562,.T.);
#9639=ORIENTED_EDGE('',*,*,#7563,.F.);
#9640=ORIENTED_EDGE('',*,*,#7562,.F.);
#9641=ORIENTED_EDGE('',*,*,#7564,.F.);
#9642=ORIENTED_EDGE('',*,*,#7565,.T.);
#9643=ORIENTED_EDGE('',*,*,#7566,.T.);
#9644=ORIENTED_EDGE('',*,*,#7565,.F.);
#9645=ORIENTED_EDGE('',*,*,#7567,.F.);
#9646=ORIENTED_EDGE('',*,*,#7568,.T.);
#9647=ORIENTED_EDGE('',*,*,#7569,.T.);
#9648=ORIENTED_EDGE('',*,*,#7568,.F.);
#9649=ORIENTED_EDGE('',*,*,#7567,.T.);
#9650=ORIENTED_EDGE('',*,*,#7564,.T.);
#9651=ORIENTED_EDGE('',*,*,#7563,.T.);
#9652=ORIENTED_EDGE('',*,*,#7560,.T.);
#9653=ORIENTED_EDGE('',*,*,#7557,.T.);
#9654=ORIENTED_EDGE('',*,*,#7554,.T.);
#9655=ORIENTED_EDGE('',*,*,#7569,.F.);
#9656=ORIENTED_EDGE('',*,*,#7566,.F.);
#9657=ORIENTED_EDGE('',*,*,#7561,.T.);
#9658=ORIENTED_EDGE('',*,*,#7558,.T.);
#9659=ORIENTED_EDGE('',*,*,#7555,.T.);
#9660=ORIENTED_EDGE('',*,*,#7552,.T.);
#9661=ORIENTED_EDGE('',*,*,#7570,.T.);
#9662=ORIENTED_EDGE('',*,*,#7571,.F.);
#9663=ORIENTED_EDGE('',*,*,#7570,.F.);
#9664=ORIENTED_EDGE('',*,*,#7572,.T.);
#9665=ORIENTED_EDGE('',*,*,#7573,.T.);
#9666=ORIENTED_EDGE('',*,*,#7572,.F.);
#9667=ORIENTED_EDGE('',*,*,#7573,.F.);
#9668=ORIENTED_EDGE('',*,*,#7574,.F.);
#9669=ORIENTED_EDGE('',*,*,#7575,.T.);
#9670=ORIENTED_EDGE('',*,*,#7571,.T.);
#9671=ORIENTED_EDGE('',*,*,#7575,.F.);
#9672=ORIENTED_EDGE('',*,*,#7574,.T.);
#9673=ORIENTED_EDGE('',*,*,#7576,.T.);
#9674=ORIENTED_EDGE('',*,*,#7577,.F.);
#9675=ORIENTED_EDGE('',*,*,#7576,.F.);
#9676=ORIENTED_EDGE('',*,*,#7578,.T.);
#9677=ORIENTED_EDGE('',*,*,#7579,.T.);
#9678=ORIENTED_EDGE('',*,*,#7578,.F.);
#9679=ORIENTED_EDGE('',*,*,#7579,.F.);
#9680=ORIENTED_EDGE('',*,*,#7580,.F.);
#9681=ORIENTED_EDGE('',*,*,#7581,.T.);
#9682=ORIENTED_EDGE('',*,*,#7577,.T.);
#9683=ORIENTED_EDGE('',*,*,#7581,.F.);
#9684=ORIENTED_EDGE('',*,*,#7580,.T.);
#9685=ORIENTED_EDGE('',*,*,#7582,.T.);
#9686=ORIENTED_EDGE('',*,*,#7583,.F.);
#9687=ORIENTED_EDGE('',*,*,#7582,.F.);
#9688=ORIENTED_EDGE('',*,*,#7584,.T.);
#9689=ORIENTED_EDGE('',*,*,#7585,.T.);
#9690=ORIENTED_EDGE('',*,*,#7584,.F.);
#9691=ORIENTED_EDGE('',*,*,#7585,.F.);
#9692=ORIENTED_EDGE('',*,*,#7586,.F.);
#9693=ORIENTED_EDGE('',*,*,#7587,.T.);
#9694=ORIENTED_EDGE('',*,*,#7583,.T.);
#9695=ORIENTED_EDGE('',*,*,#7587,.F.);
#9696=ORIENTED_EDGE('',*,*,#7586,.T.);
#9697=ORIENTED_EDGE('',*,*,#7588,.T.);
#9698=ORIENTED_EDGE('',*,*,#7589,.F.);
#9699=ORIENTED_EDGE('',*,*,#7588,.F.);
#9700=ORIENTED_EDGE('',*,*,#7590,.T.);
#9701=ORIENTED_EDGE('',*,*,#7591,.T.);
#9702=ORIENTED_EDGE('',*,*,#7590,.F.);
#9703=ORIENTED_EDGE('',*,*,#7591,.F.);
#9704=ORIENTED_EDGE('',*,*,#7592,.F.);
#9705=ORIENTED_EDGE('',*,*,#7593,.T.);
#9706=ORIENTED_EDGE('',*,*,#7589,.T.);
#9707=ORIENTED_EDGE('',*,*,#7593,.F.);
#9708=ORIENTED_EDGE('',*,*,#7592,.T.);
#9709=ORIENTED_EDGE('',*,*,#7594,.F.);
#9710=ORIENTED_EDGE('',*,*,#7595,.T.);
#9711=ORIENTED_EDGE('',*,*,#7596,.F.);
#9712=ORIENTED_EDGE('',*,*,#7595,.F.);
#9713=ORIENTED_EDGE('',*,*,#7597,.F.);
#9714=ORIENTED_EDGE('',*,*,#7598,.T.);
#9715=ORIENTED_EDGE('',*,*,#7599,.F.);
#9716=ORIENTED_EDGE('',*,*,#7598,.F.);
#9717=ORIENTED_EDGE('',*,*,#7600,.F.);
#9718=ORIENTED_EDGE('',*,*,#7601,.T.);
#9719=ORIENTED_EDGE('',*,*,#7602,.F.);
#9720=ORIENTED_EDGE('',*,*,#7601,.F.);
#9721=ORIENTED_EDGE('',*,*,#7603,.F.);
#9722=ORIENTED_EDGE('',*,*,#7604,.T.);
#9723=ORIENTED_EDGE('',*,*,#7605,.F.);
#9724=ORIENTED_EDGE('',*,*,#7604,.F.);
#9725=ORIENTED_EDGE('',*,*,#7606,.F.);
#9726=ORIENTED_EDGE('',*,*,#7607,.T.);
#9727=ORIENTED_EDGE('',*,*,#7608,.T.);
#9728=ORIENTED_EDGE('',*,*,#7607,.F.);
#9729=ORIENTED_EDGE('',*,*,#7609,.F.);
#9730=ORIENTED_EDGE('',*,*,#7610,.T.);
#9731=ORIENTED_EDGE('',*,*,#7611,.T.);
#9732=ORIENTED_EDGE('',*,*,#7610,.F.);
#9733=ORIENTED_EDGE('',*,*,#7609,.T.);
#9734=ORIENTED_EDGE('',*,*,#7606,.T.);
#9735=ORIENTED_EDGE('',*,*,#7605,.T.);
#9736=ORIENTED_EDGE('',*,*,#7602,.T.);
#9737=ORIENTED_EDGE('',*,*,#7599,.T.);
#9738=ORIENTED_EDGE('',*,*,#7596,.T.);
#9739=ORIENTED_EDGE('',*,*,#7611,.F.);
#9740=ORIENTED_EDGE('',*,*,#7608,.F.);
#9741=ORIENTED_EDGE('',*,*,#7603,.T.);
#9742=ORIENTED_EDGE('',*,*,#7600,.T.);
#9743=ORIENTED_EDGE('',*,*,#7597,.T.);
#9744=ORIENTED_EDGE('',*,*,#7594,.T.);
#9745=ORIENTED_EDGE('',*,*,#7612,.F.);
#9746=ORIENTED_EDGE('',*,*,#7613,.T.);
#9747=ORIENTED_EDGE('',*,*,#7614,.F.);
#9748=ORIENTED_EDGE('',*,*,#7615,.T.);
#9749=ORIENTED_EDGE('',*,*,#7612,.T.);
#9750=ORIENTED_EDGE('',*,*,#7615,.F.);
#9751=ORIENTED_EDGE('',*,*,#7614,.T.);
#9752=ORIENTED_EDGE('',*,*,#7613,.F.);
#9753=ORIENTED_EDGE('',*,*,#7616,.T.);
#9754=ORIENTED_EDGE('',*,*,#7617,.T.);
#9755=ORIENTED_EDGE('',*,*,#7616,.F.);
#9756=ORIENTED_EDGE('',*,*,#7617,.F.);
#9757=ORIENTED_EDGE('',*,*,#7618,.F.);
#9758=ORIENTED_EDGE('',*,*,#7619,.T.);
#9759=ORIENTED_EDGE('',*,*,#7620,.F.);
#9760=ORIENTED_EDGE('',*,*,#7621,.T.);
#9761=ORIENTED_EDGE('',*,*,#7618,.T.);
#9762=ORIENTED_EDGE('',*,*,#7621,.F.);
#9763=ORIENTED_EDGE('',*,*,#7620,.T.);
#9764=ORIENTED_EDGE('',*,*,#7619,.F.);
#9765=ORIENTED_EDGE('',*,*,#7622,.T.);
#9766=ORIENTED_EDGE('',*,*,#7623,.T.);
#9767=ORIENTED_EDGE('',*,*,#7622,.F.);
#9768=ORIENTED_EDGE('',*,*,#7623,.F.);
#9769=ORIENTED_EDGE('',*,*,#7624,.F.);
#9770=ORIENTED_EDGE('',*,*,#7625,.T.);
#9771=ORIENTED_EDGE('',*,*,#7626,.F.);
#9772=ORIENTED_EDGE('',*,*,#7627,.T.);
#9773=ORIENTED_EDGE('',*,*,#7624,.T.);
#9774=ORIENTED_EDGE('',*,*,#7627,.F.);
#9775=ORIENTED_EDGE('',*,*,#7626,.T.);
#9776=ORIENTED_EDGE('',*,*,#7625,.F.);
#9777=ORIENTED_EDGE('',*,*,#7628,.T.);
#9778=ORIENTED_EDGE('',*,*,#7629,.T.);
#9779=ORIENTED_EDGE('',*,*,#7628,.F.);
#9780=ORIENTED_EDGE('',*,*,#7629,.F.);
#9781=ORIENTED_EDGE('',*,*,#7630,.F.);
#9782=ORIENTED_EDGE('',*,*,#7631,.T.);
#9783=ORIENTED_EDGE('',*,*,#7632,.F.);
#9784=ORIENTED_EDGE('',*,*,#7633,.T.);
#9785=ORIENTED_EDGE('',*,*,#7630,.T.);
#9786=ORIENTED_EDGE('',*,*,#7633,.F.);
#9787=ORIENTED_EDGE('',*,*,#7632,.T.);
#9788=ORIENTED_EDGE('',*,*,#7631,.F.);
#9789=ORIENTED_EDGE('',*,*,#7634,.T.);
#9790=ORIENTED_EDGE('',*,*,#7635,.T.);
#9791=ORIENTED_EDGE('',*,*,#7634,.F.);
#9792=ORIENTED_EDGE('',*,*,#7635,.F.);
#9793=ORIENTED_EDGE('',*,*,#7636,.F.);
#9794=ORIENTED_EDGE('',*,*,#7637,.T.);
#9795=ORIENTED_EDGE('',*,*,#7638,.F.);
#9796=ORIENTED_EDGE('',*,*,#7637,.F.);
#9797=ORIENTED_EDGE('',*,*,#7639,.F.);
#9798=ORIENTED_EDGE('',*,*,#7640,.T.);
#9799=ORIENTED_EDGE('',*,*,#7641,.F.);
#9800=ORIENTED_EDGE('',*,*,#7640,.F.);
#9801=ORIENTED_EDGE('',*,*,#7642,.F.);
#9802=ORIENTED_EDGE('',*,*,#7643,.T.);
#9803=ORIENTED_EDGE('',*,*,#7644,.F.);
#9804=ORIENTED_EDGE('',*,*,#7643,.F.);
#9805=ORIENTED_EDGE('',*,*,#7645,.F.);
#9806=ORIENTED_EDGE('',*,*,#7646,.T.);
#9807=ORIENTED_EDGE('',*,*,#7647,.F.);
#9808=ORIENTED_EDGE('',*,*,#7646,.F.);
#9809=ORIENTED_EDGE('',*,*,#7648,.F.);
#9810=ORIENTED_EDGE('',*,*,#7649,.T.);
#9811=ORIENTED_EDGE('',*,*,#7650,.F.);
#9812=ORIENTED_EDGE('',*,*,#7649,.F.);
#9813=ORIENTED_EDGE('',*,*,#7651,.F.);
#9814=ORIENTED_EDGE('',*,*,#7652,.T.);
#9815=ORIENTED_EDGE('',*,*,#7653,.F.);
#9816=ORIENTED_EDGE('',*,*,#7654,.F.);
#9817=ORIENTED_EDGE('',*,*,#7651,.T.);
#9818=ORIENTED_EDGE('',*,*,#7655,.F.);
#9819=ORIENTED_EDGE('',*,*,#7656,.T.);
#9820=ORIENTED_EDGE('',*,*,#7657,.T.);
#9821=ORIENTED_EDGE('',*,*,#7654,.T.);
#9822=ORIENTED_EDGE('',*,*,#7658,.T.);
#9823=ORIENTED_EDGE('',*,*,#7659,.T.);
#9824=ORIENTED_EDGE('',*,*,#7655,.T.);
#9825=ORIENTED_EDGE('',*,*,#7660,.T.);
#9826=ORIENTED_EDGE('',*,*,#7661,.T.);
#9827=ORIENTED_EDGE('',*,*,#7662,.T.);
#9828=ORIENTED_EDGE('',*,*,#7663,.T.);
#9829=ORIENTED_EDGE('',*,*,#7664,.T.);
#9830=ORIENTED_EDGE('',*,*,#7650,.T.);
#9831=ORIENTED_EDGE('',*,*,#7647,.T.);
#9832=ORIENTED_EDGE('',*,*,#7644,.T.);
#9833=ORIENTED_EDGE('',*,*,#7641,.T.);
#9834=ORIENTED_EDGE('',*,*,#7638,.T.);
#9835=ORIENTED_EDGE('',*,*,#7665,.F.);
#9836=ORIENTED_EDGE('',*,*,#7666,.T.);
#9837=ORIENTED_EDGE('',*,*,#7664,.F.);
#9838=ORIENTED_EDGE('',*,*,#7666,.F.);
#9839=ORIENTED_EDGE('',*,*,#7667,.F.);
#9840=ORIENTED_EDGE('',*,*,#7668,.T.);
#9841=ORIENTED_EDGE('',*,*,#7663,.F.);
#9842=ORIENTED_EDGE('',*,*,#7668,.F.);
#9843=ORIENTED_EDGE('',*,*,#7669,.F.);
#9844=ORIENTED_EDGE('',*,*,#7670,.T.);
#9845=ORIENTED_EDGE('',*,*,#7662,.F.);
#9846=ORIENTED_EDGE('',*,*,#7670,.F.);
#9847=ORIENTED_EDGE('',*,*,#7671,.F.);
#9848=ORIENTED_EDGE('',*,*,#7672,.T.);
#9849=ORIENTED_EDGE('',*,*,#7661,.F.);
#9850=ORIENTED_EDGE('',*,*,#7672,.F.);
#9851=ORIENTED_EDGE('',*,*,#7673,.F.);
#9852=ORIENTED_EDGE('',*,*,#7674,.T.);
#9853=ORIENTED_EDGE('',*,*,#7660,.F.);
#9854=ORIENTED_EDGE('',*,*,#7674,.F.);
#9855=ORIENTED_EDGE('',*,*,#7675,.F.);
#9856=ORIENTED_EDGE('',*,*,#7676,.T.);
#9857=ORIENTED_EDGE('',*,*,#7656,.F.);
#9858=ORIENTED_EDGE('',*,*,#7659,.F.);
#9859=ORIENTED_EDGE('',*,*,#7653,.T.);
#9860=ORIENTED_EDGE('',*,*,#7677,.T.);
#9861=ORIENTED_EDGE('',*,*,#7675,.T.);
#9862=ORIENTED_EDGE('',*,*,#7658,.F.);
#9863=ORIENTED_EDGE('',*,*,#7657,.F.);
#9864=ORIENTED_EDGE('',*,*,#7676,.F.);
#9865=ORIENTED_EDGE('',*,*,#7677,.F.);
#9866=ORIENTED_EDGE('',*,*,#7652,.F.);
#9867=ORIENTED_EDGE('',*,*,#7665,.T.);
#9868=ORIENTED_EDGE('',*,*,#7667,.T.);
#9869=ORIENTED_EDGE('',*,*,#7669,.T.);
#9870=ORIENTED_EDGE('',*,*,#7671,.T.);
#9871=ORIENTED_EDGE('',*,*,#7673,.T.);
#9872=ORIENTED_EDGE('',*,*,#7648,.T.);
#9873=ORIENTED_EDGE('',*,*,#7645,.T.);
#9874=ORIENTED_EDGE('',*,*,#7642,.T.);
#9875=ORIENTED_EDGE('',*,*,#7639,.T.);
#9876=ORIENTED_EDGE('',*,*,#7636,.T.);
#9877=ORIENTED_EDGE('',*,*,#7678,.F.);
#9878=ORIENTED_EDGE('',*,*,#7679,.T.);
#9879=ORIENTED_EDGE('',*,*,#7680,.F.);
#9880=ORIENTED_EDGE('',*,*,#7679,.F.);
#9881=ORIENTED_EDGE('',*,*,#7681,.F.);
#9882=ORIENTED_EDGE('',*,*,#7682,.T.);
#9883=ORIENTED_EDGE('',*,*,#7683,.F.);
#9884=ORIENTED_EDGE('',*,*,#7682,.F.);
#9885=ORIENTED_EDGE('',*,*,#7684,.F.);
#9886=ORIENTED_EDGE('',*,*,#7685,.T.);
#9887=ORIENTED_EDGE('',*,*,#7686,.F.);
#9888=ORIENTED_EDGE('',*,*,#7685,.F.);
#9889=ORIENTED_EDGE('',*,*,#7687,.F.);
#9890=ORIENTED_EDGE('',*,*,#7688,.T.);
#9891=ORIENTED_EDGE('',*,*,#7689,.F.);
#9892=ORIENTED_EDGE('',*,*,#7688,.F.);
#9893=ORIENTED_EDGE('',*,*,#7690,.F.);
#9894=ORIENTED_EDGE('',*,*,#7691,.T.);
#9895=ORIENTED_EDGE('',*,*,#7692,.T.);
#9896=ORIENTED_EDGE('',*,*,#7691,.F.);
#9897=ORIENTED_EDGE('',*,*,#7693,.F.);
#9898=ORIENTED_EDGE('',*,*,#7694,.T.);
#9899=ORIENTED_EDGE('',*,*,#7695,.T.);
#9900=ORIENTED_EDGE('',*,*,#7694,.F.);
#9901=ORIENTED_EDGE('',*,*,#7693,.T.);
#9902=ORIENTED_EDGE('',*,*,#7690,.T.);
#9903=ORIENTED_EDGE('',*,*,#7689,.T.);
#9904=ORIENTED_EDGE('',*,*,#7686,.T.);
#9905=ORIENTED_EDGE('',*,*,#7683,.T.);
#9906=ORIENTED_EDGE('',*,*,#7680,.T.);
#9907=ORIENTED_EDGE('',*,*,#7695,.F.);
#9908=ORIENTED_EDGE('',*,*,#7692,.F.);
#9909=ORIENTED_EDGE('',*,*,#7687,.T.);
#9910=ORIENTED_EDGE('',*,*,#7684,.T.);
#9911=ORIENTED_EDGE('',*,*,#7681,.T.);
#9912=ORIENTED_EDGE('',*,*,#7678,.T.);
#9913=ORIENTED_EDGE('',*,*,#7696,.T.);
#9914=ORIENTED_EDGE('',*,*,#7697,.F.);
#9915=ORIENTED_EDGE('',*,*,#7696,.F.);
#9916=ORIENTED_EDGE('',*,*,#7698,.T.);
#9917=ORIENTED_EDGE('',*,*,#7699,.T.);
#9918=ORIENTED_EDGE('',*,*,#7698,.F.);
#9919=ORIENTED_EDGE('',*,*,#7699,.F.);
#9920=ORIENTED_EDGE('',*,*,#7700,.F.);
#9921=ORIENTED_EDGE('',*,*,#7701,.T.);
#9922=ORIENTED_EDGE('',*,*,#7697,.T.);
#9923=ORIENTED_EDGE('',*,*,#7701,.F.);
#9924=ORIENTED_EDGE('',*,*,#7700,.T.);
#9925=ORIENTED_EDGE('',*,*,#7702,.T.);
#9926=ORIENTED_EDGE('',*,*,#7703,.F.);
#9927=ORIENTED_EDGE('',*,*,#7702,.F.);
#9928=ORIENTED_EDGE('',*,*,#7704,.T.);
#9929=ORIENTED_EDGE('',*,*,#7705,.T.);
#9930=ORIENTED_EDGE('',*,*,#7704,.F.);
#9931=ORIENTED_EDGE('',*,*,#7705,.F.);
#9932=ORIENTED_EDGE('',*,*,#7706,.F.);
#9933=ORIENTED_EDGE('',*,*,#7707,.T.);
#9934=ORIENTED_EDGE('',*,*,#7703,.T.);
#9935=ORIENTED_EDGE('',*,*,#7707,.F.);
#9936=ORIENTED_EDGE('',*,*,#7706,.T.);
#9937=ORIENTED_EDGE('',*,*,#7708,.T.);
#9938=ORIENTED_EDGE('',*,*,#7709,.F.);
#9939=ORIENTED_EDGE('',*,*,#7708,.F.);
#9940=ORIENTED_EDGE('',*,*,#7710,.T.);
#9941=ORIENTED_EDGE('',*,*,#7711,.T.);
#9942=ORIENTED_EDGE('',*,*,#7710,.F.);
#9943=ORIENTED_EDGE('',*,*,#7711,.F.);
#9944=ORIENTED_EDGE('',*,*,#7712,.F.);
#9945=ORIENTED_EDGE('',*,*,#7713,.T.);
#9946=ORIENTED_EDGE('',*,*,#7709,.T.);
#9947=ORIENTED_EDGE('',*,*,#7713,.F.);
#9948=ORIENTED_EDGE('',*,*,#7712,.T.);
#9949=ORIENTED_EDGE('',*,*,#7714,.T.);
#9950=ORIENTED_EDGE('',*,*,#7715,.F.);
#9951=ORIENTED_EDGE('',*,*,#7714,.F.);
#9952=ORIENTED_EDGE('',*,*,#7716,.T.);
#9953=ORIENTED_EDGE('',*,*,#7717,.T.);
#9954=ORIENTED_EDGE('',*,*,#7716,.F.);
#9955=ORIENTED_EDGE('',*,*,#7717,.F.);
#9956=ORIENTED_EDGE('',*,*,#7718,.F.);
#9957=ORIENTED_EDGE('',*,*,#7719,.T.);
#9958=ORIENTED_EDGE('',*,*,#7715,.T.);
#9959=ORIENTED_EDGE('',*,*,#7719,.F.);
#9960=ORIENTED_EDGE('',*,*,#7718,.T.);
#9961=ORIENTED_EDGE('',*,*,#7720,.F.);
#9962=ORIENTED_EDGE('',*,*,#7721,.T.);
#9963=ORIENTED_EDGE('',*,*,#7722,.F.);
#9964=ORIENTED_EDGE('',*,*,#7721,.F.);
#9965=ORIENTED_EDGE('',*,*,#7723,.F.);
#9966=ORIENTED_EDGE('',*,*,#7724,.T.);
#9967=ORIENTED_EDGE('',*,*,#7725,.F.);
#9968=ORIENTED_EDGE('',*,*,#7724,.F.);
#9969=ORIENTED_EDGE('',*,*,#7726,.F.);
#9970=ORIENTED_EDGE('',*,*,#7727,.T.);
#9971=ORIENTED_EDGE('',*,*,#7728,.F.);
#9972=ORIENTED_EDGE('',*,*,#7727,.F.);
#9973=ORIENTED_EDGE('',*,*,#7729,.F.);
#9974=ORIENTED_EDGE('',*,*,#7730,.T.);
#9975=ORIENTED_EDGE('',*,*,#7731,.F.);
#9976=ORIENTED_EDGE('',*,*,#7730,.F.);
#9977=ORIENTED_EDGE('',*,*,#7732,.F.);
#9978=ORIENTED_EDGE('',*,*,#7733,.T.);
#9979=ORIENTED_EDGE('',*,*,#7734,.T.);
#9980=ORIENTED_EDGE('',*,*,#7733,.F.);
#9981=ORIENTED_EDGE('',*,*,#7735,.F.);
#9982=ORIENTED_EDGE('',*,*,#7736,.T.);
#9983=ORIENTED_EDGE('',*,*,#7737,.T.);
#9984=ORIENTED_EDGE('',*,*,#7736,.F.);
#9985=ORIENTED_EDGE('',*,*,#7735,.T.);
#9986=ORIENTED_EDGE('',*,*,#7732,.T.);
#9987=ORIENTED_EDGE('',*,*,#7731,.T.);
#9988=ORIENTED_EDGE('',*,*,#7728,.T.);
#9989=ORIENTED_EDGE('',*,*,#7725,.T.);
#9990=ORIENTED_EDGE('',*,*,#7722,.T.);
#9991=ORIENTED_EDGE('',*,*,#7737,.F.);
#9992=ORIENTED_EDGE('',*,*,#7734,.F.);
#9993=ORIENTED_EDGE('',*,*,#7729,.T.);
#9994=ORIENTED_EDGE('',*,*,#7726,.T.);
#9995=ORIENTED_EDGE('',*,*,#7723,.T.);
#9996=ORIENTED_EDGE('',*,*,#7720,.T.);
#9997=ORIENTED_EDGE('',*,*,#7738,.F.);
#9998=ORIENTED_EDGE('',*,*,#7739,.T.);
#9999=ORIENTED_EDGE('',*,*,#7740,.F.);
#10000=ORIENTED_EDGE('',*,*,#7741,.T.);
#10001=ORIENTED_EDGE('',*,*,#7738,.T.);
#10002=ORIENTED_EDGE('',*,*,#7741,.F.);
#10003=ORIENTED_EDGE('',*,*,#7740,.T.);
#10004=ORIENTED_EDGE('',*,*,#7739,.F.);
#10005=ORIENTED_EDGE('',*,*,#7742,.T.);
#10006=ORIENTED_EDGE('',*,*,#7743,.T.);
#10007=ORIENTED_EDGE('',*,*,#7742,.F.);
#10008=ORIENTED_EDGE('',*,*,#7743,.F.);
#10009=ORIENTED_EDGE('',*,*,#7744,.F.);
#10010=ORIENTED_EDGE('',*,*,#7745,.T.);
#10011=ORIENTED_EDGE('',*,*,#7746,.F.);
#10012=ORIENTED_EDGE('',*,*,#7747,.T.);
#10013=ORIENTED_EDGE('',*,*,#7744,.T.);
#10014=ORIENTED_EDGE('',*,*,#7747,.F.);
#10015=ORIENTED_EDGE('',*,*,#7746,.T.);
#10016=ORIENTED_EDGE('',*,*,#7745,.F.);
#10017=ORIENTED_EDGE('',*,*,#7748,.T.);
#10018=ORIENTED_EDGE('',*,*,#7749,.T.);
#10019=ORIENTED_EDGE('',*,*,#7748,.F.);
#10020=ORIENTED_EDGE('',*,*,#7749,.F.);
#10021=ORIENTED_EDGE('',*,*,#7750,.F.);
#10022=ORIENTED_EDGE('',*,*,#7751,.T.);
#10023=ORIENTED_EDGE('',*,*,#7752,.F.);
#10024=ORIENTED_EDGE('',*,*,#7753,.T.);
#10025=ORIENTED_EDGE('',*,*,#7750,.T.);
#10026=ORIENTED_EDGE('',*,*,#7753,.F.);
#10027=ORIENTED_EDGE('',*,*,#7752,.T.);
#10028=ORIENTED_EDGE('',*,*,#7751,.F.);
#10029=ORIENTED_EDGE('',*,*,#7754,.T.);
#10030=ORIENTED_EDGE('',*,*,#7755,.T.);
#10031=ORIENTED_EDGE('',*,*,#7754,.F.);
#10032=ORIENTED_EDGE('',*,*,#7755,.F.);
#10033=ORIENTED_EDGE('',*,*,#7756,.F.);
#10034=ORIENTED_EDGE('',*,*,#7757,.T.);
#10035=ORIENTED_EDGE('',*,*,#7758,.F.);
#10036=ORIENTED_EDGE('',*,*,#7759,.T.);
#10037=ORIENTED_EDGE('',*,*,#7756,.T.);
#10038=ORIENTED_EDGE('',*,*,#7759,.F.);
#10039=ORIENTED_EDGE('',*,*,#7758,.T.);
#10040=ORIENTED_EDGE('',*,*,#7757,.F.);
#10041=ORIENTED_EDGE('',*,*,#7760,.T.);
#10042=ORIENTED_EDGE('',*,*,#7761,.T.);
#10043=ORIENTED_EDGE('',*,*,#7760,.F.);
#10044=ORIENTED_EDGE('',*,*,#7761,.F.);
#10045=ORIENTED_EDGE('',*,*,#7762,.F.);
#10046=ORIENTED_EDGE('',*,*,#7763,.T.);
#10047=ORIENTED_EDGE('',*,*,#7764,.F.);
#10048=ORIENTED_EDGE('',*,*,#7763,.F.);
#10049=ORIENTED_EDGE('',*,*,#7765,.F.);
#10050=ORIENTED_EDGE('',*,*,#7766,.T.);
#10051=ORIENTED_EDGE('',*,*,#7767,.F.);
#10052=ORIENTED_EDGE('',*,*,#7766,.F.);
#10053=ORIENTED_EDGE('',*,*,#7768,.F.);
#10054=ORIENTED_EDGE('',*,*,#7769,.T.);
#10055=ORIENTED_EDGE('',*,*,#7770,.F.);
#10056=ORIENTED_EDGE('',*,*,#7769,.F.);
#10057=ORIENTED_EDGE('',*,*,#7771,.F.);
#10058=ORIENTED_EDGE('',*,*,#7772,.T.);
#10059=ORIENTED_EDGE('',*,*,#7773,.F.);
#10060=ORIENTED_EDGE('',*,*,#7772,.F.);
#10061=ORIENTED_EDGE('',*,*,#7774,.F.);
#10062=ORIENTED_EDGE('',*,*,#7775,.T.);
#10063=ORIENTED_EDGE('',*,*,#7776,.T.);
#10064=ORIENTED_EDGE('',*,*,#7775,.F.);
#10065=ORIENTED_EDGE('',*,*,#7777,.F.);
#10066=ORIENTED_EDGE('',*,*,#7778,.T.);
#10067=ORIENTED_EDGE('',*,*,#7779,.T.);
#10068=ORIENTED_EDGE('',*,*,#7778,.F.);
#10069=ORIENTED_EDGE('',*,*,#7777,.T.);
#10070=ORIENTED_EDGE('',*,*,#7774,.T.);
#10071=ORIENTED_EDGE('',*,*,#7773,.T.);
#10072=ORIENTED_EDGE('',*,*,#7770,.T.);
#10073=ORIENTED_EDGE('',*,*,#7767,.T.);
#10074=ORIENTED_EDGE('',*,*,#7764,.T.);
#10075=ORIENTED_EDGE('',*,*,#7779,.F.);
#10076=ORIENTED_EDGE('',*,*,#7776,.F.);
#10077=ORIENTED_EDGE('',*,*,#7771,.T.);
#10078=ORIENTED_EDGE('',*,*,#7768,.T.);
#10079=ORIENTED_EDGE('',*,*,#7765,.T.);
#10080=ORIENTED_EDGE('',*,*,#7762,.T.);
#10081=ORIENTED_EDGE('',*,*,#7780,.T.);
#10082=ORIENTED_EDGE('',*,*,#7781,.F.);
#10083=ORIENTED_EDGE('',*,*,#7780,.F.);
#10084=ORIENTED_EDGE('',*,*,#7782,.T.);
#10085=ORIENTED_EDGE('',*,*,#7783,.T.);
#10086=ORIENTED_EDGE('',*,*,#7782,.F.);
#10087=ORIENTED_EDGE('',*,*,#7783,.F.);
#10088=ORIENTED_EDGE('',*,*,#7784,.F.);
#10089=ORIENTED_EDGE('',*,*,#7785,.T.);
#10090=ORIENTED_EDGE('',*,*,#7781,.T.);
#10091=ORIENTED_EDGE('',*,*,#7785,.F.);
#10092=ORIENTED_EDGE('',*,*,#7784,.T.);
#10093=ORIENTED_EDGE('',*,*,#7786,.T.);
#10094=ORIENTED_EDGE('',*,*,#7787,.F.);
#10095=ORIENTED_EDGE('',*,*,#7786,.F.);
#10096=ORIENTED_EDGE('',*,*,#7788,.T.);
#10097=ORIENTED_EDGE('',*,*,#7789,.T.);
#10098=ORIENTED_EDGE('',*,*,#7788,.F.);
#10099=ORIENTED_EDGE('',*,*,#7789,.F.);
#10100=ORIENTED_EDGE('',*,*,#7790,.F.);
#10101=ORIENTED_EDGE('',*,*,#7791,.T.);
#10102=ORIENTED_EDGE('',*,*,#7787,.T.);
#10103=ORIENTED_EDGE('',*,*,#7791,.F.);
#10104=ORIENTED_EDGE('',*,*,#7790,.T.);
#10105=ORIENTED_EDGE('',*,*,#7792,.T.);
#10106=ORIENTED_EDGE('',*,*,#7793,.F.);
#10107=ORIENTED_EDGE('',*,*,#7792,.F.);
#10108=ORIENTED_EDGE('',*,*,#7794,.T.);
#10109=ORIENTED_EDGE('',*,*,#7795,.T.);
#10110=ORIENTED_EDGE('',*,*,#7794,.F.);
#10111=ORIENTED_EDGE('',*,*,#7795,.F.);
#10112=ORIENTED_EDGE('',*,*,#7796,.F.);
#10113=ORIENTED_EDGE('',*,*,#7797,.T.);
#10114=ORIENTED_EDGE('',*,*,#7793,.T.);
#10115=ORIENTED_EDGE('',*,*,#7797,.F.);
#10116=ORIENTED_EDGE('',*,*,#7796,.T.);
#10117=ORIENTED_EDGE('',*,*,#7798,.T.);
#10118=ORIENTED_EDGE('',*,*,#7799,.F.);
#10119=ORIENTED_EDGE('',*,*,#7798,.F.);
#10120=ORIENTED_EDGE('',*,*,#7800,.T.);
#10121=ORIENTED_EDGE('',*,*,#7801,.T.);
#10122=ORIENTED_EDGE('',*,*,#7800,.F.);
#10123=ORIENTED_EDGE('',*,*,#7801,.F.);
#10124=ORIENTED_EDGE('',*,*,#7802,.F.);
#10125=ORIENTED_EDGE('',*,*,#7803,.T.);
#10126=ORIENTED_EDGE('',*,*,#7799,.T.);
#10127=ORIENTED_EDGE('',*,*,#7803,.F.);
#10128=ORIENTED_EDGE('',*,*,#7802,.T.);
#10129=ORIENTED_EDGE('',*,*,#7804,.F.);
#10130=ORIENTED_EDGE('',*,*,#7805,.T.);
#10131=ORIENTED_EDGE('',*,*,#7806,.F.);
#10132=ORIENTED_EDGE('',*,*,#7805,.F.);
#10133=ORIENTED_EDGE('',*,*,#7807,.F.);
#10134=ORIENTED_EDGE('',*,*,#7808,.T.);
#10135=ORIENTED_EDGE('',*,*,#7809,.F.);
#10136=ORIENTED_EDGE('',*,*,#7808,.F.);
#10137=ORIENTED_EDGE('',*,*,#7810,.F.);
#10138=ORIENTED_EDGE('',*,*,#7811,.T.);
#10139=ORIENTED_EDGE('',*,*,#7812,.F.);
#10140=ORIENTED_EDGE('',*,*,#7811,.F.);
#10141=ORIENTED_EDGE('',*,*,#7813,.F.);
#10142=ORIENTED_EDGE('',*,*,#7814,.T.);
#10143=ORIENTED_EDGE('',*,*,#7815,.F.);
#10144=ORIENTED_EDGE('',*,*,#7814,.F.);
#10145=ORIENTED_EDGE('',*,*,#7816,.F.);
#10146=ORIENTED_EDGE('',*,*,#7817,.T.);
#10147=ORIENTED_EDGE('',*,*,#7818,.T.);
#10148=ORIENTED_EDGE('',*,*,#7817,.F.);
#10149=ORIENTED_EDGE('',*,*,#7819,.F.);
#10150=ORIENTED_EDGE('',*,*,#7820,.T.);
#10151=ORIENTED_EDGE('',*,*,#7821,.T.);
#10152=ORIENTED_EDGE('',*,*,#7820,.F.);
#10153=ORIENTED_EDGE('',*,*,#7819,.T.);
#10154=ORIENTED_EDGE('',*,*,#7816,.T.);
#10155=ORIENTED_EDGE('',*,*,#7815,.T.);
#10156=ORIENTED_EDGE('',*,*,#7812,.T.);
#10157=ORIENTED_EDGE('',*,*,#7809,.T.);
#10158=ORIENTED_EDGE('',*,*,#7806,.T.);
#10159=ORIENTED_EDGE('',*,*,#7821,.F.);
#10160=ORIENTED_EDGE('',*,*,#7818,.F.);
#10161=ORIENTED_EDGE('',*,*,#7813,.T.);
#10162=ORIENTED_EDGE('',*,*,#7810,.T.);
#10163=ORIENTED_EDGE('',*,*,#7807,.T.);
#10164=ORIENTED_EDGE('',*,*,#7804,.T.);
#10165=ORIENTED_EDGE('',*,*,#7822,.F.);
#10166=ORIENTED_EDGE('',*,*,#7823,.T.);
#10167=ORIENTED_EDGE('',*,*,#7824,.F.);
#10168=ORIENTED_EDGE('',*,*,#7825,.T.);
#10169=ORIENTED_EDGE('',*,*,#7822,.T.);
#10170=ORIENTED_EDGE('',*,*,#7825,.F.);
#10171=ORIENTED_EDGE('',*,*,#7824,.T.);
#10172=ORIENTED_EDGE('',*,*,#7823,.F.);
#10173=ORIENTED_EDGE('',*,*,#7826,.T.);
#10174=ORIENTED_EDGE('',*,*,#7827,.T.);
#10175=ORIENTED_EDGE('',*,*,#7826,.F.);
#10176=ORIENTED_EDGE('',*,*,#7827,.F.);
#10177=ORIENTED_EDGE('',*,*,#7828,.F.);
#10178=ORIENTED_EDGE('',*,*,#7829,.T.);
#10179=ORIENTED_EDGE('',*,*,#7830,.F.);
#10180=ORIENTED_EDGE('',*,*,#7831,.T.);
#10181=ORIENTED_EDGE('',*,*,#7828,.T.);
#10182=ORIENTED_EDGE('',*,*,#7831,.F.);
#10183=ORIENTED_EDGE('',*,*,#7830,.T.);
#10184=ORIENTED_EDGE('',*,*,#7829,.F.);
#10185=ORIENTED_EDGE('',*,*,#7832,.T.);
#10186=ORIENTED_EDGE('',*,*,#7833,.T.);
#10187=ORIENTED_EDGE('',*,*,#7832,.F.);
#10188=ORIENTED_EDGE('',*,*,#7833,.F.);
#10189=ORIENTED_EDGE('',*,*,#7834,.F.);
#10190=ORIENTED_EDGE('',*,*,#7835,.T.);
#10191=ORIENTED_EDGE('',*,*,#7836,.F.);
#10192=ORIENTED_EDGE('',*,*,#7837,.T.);
#10193=ORIENTED_EDGE('',*,*,#7834,.T.);
#10194=ORIENTED_EDGE('',*,*,#7837,.F.);
#10195=ORIENTED_EDGE('',*,*,#7836,.T.);
#10196=ORIENTED_EDGE('',*,*,#7835,.F.);
#10197=ORIENTED_EDGE('',*,*,#7838,.T.);
#10198=ORIENTED_EDGE('',*,*,#7839,.T.);
#10199=ORIENTED_EDGE('',*,*,#7838,.F.);
#10200=ORIENTED_EDGE('',*,*,#7839,.F.);
#10201=ORIENTED_EDGE('',*,*,#7840,.F.);
#10202=ORIENTED_EDGE('',*,*,#7841,.T.);
#10203=ORIENTED_EDGE('',*,*,#7842,.F.);
#10204=ORIENTED_EDGE('',*,*,#7843,.T.);
#10205=ORIENTED_EDGE('',*,*,#7840,.T.);
#10206=ORIENTED_EDGE('',*,*,#7843,.F.);
#10207=ORIENTED_EDGE('',*,*,#7842,.T.);
#10208=ORIENTED_EDGE('',*,*,#7841,.F.);
#10209=ORIENTED_EDGE('',*,*,#7844,.T.);
#10210=ORIENTED_EDGE('',*,*,#7845,.T.);
#10211=ORIENTED_EDGE('',*,*,#7844,.F.);
#10212=ORIENTED_EDGE('',*,*,#7845,.F.);
#10213=ORIENTED_EDGE('',*,*,#7846,.F.);
#10214=ORIENTED_EDGE('',*,*,#7847,.F.);
#10215=ORIENTED_EDGE('',*,*,#7848,.T.);
#10216=ORIENTED_EDGE('',*,*,#7849,.F.);
#10217=ORIENTED_EDGE('',*,*,#7850,.F.);
#10218=ORIENTED_EDGE('',*,*,#7848,.F.);
#10219=ORIENTED_EDGE('',*,*,#7849,.T.);
#10220=ORIENTED_EDGE('',*,*,#7850,.T.);
#10221=ORIENTED_EDGE('',*,*,#7851,.T.);
#10222=ORIENTED_EDGE('',*,*,#7852,.T.);
#10223=ORIENTED_EDGE('',*,*,#7851,.F.);
#10224=ORIENTED_EDGE('',*,*,#7853,.T.);
#10225=ORIENTED_EDGE('',*,*,#7854,.T.);
#10226=ORIENTED_EDGE('',*,*,#7855,.F.);
#10227=ORIENTED_EDGE('',*,*,#7854,.F.);
#10228=ORIENTED_EDGE('',*,*,#7855,.T.);
#10229=ORIENTED_EDGE('',*,*,#7856,.T.);
#10230=ORIENTED_EDGE('',*,*,#7857,.F.);
#10231=ORIENTED_EDGE('',*,*,#7856,.F.);
#10232=ORIENTED_EDGE('',*,*,#7852,.F.);
#10233=ORIENTED_EDGE('',*,*,#7857,.T.);
#10234=ORIENTED_EDGE('',*,*,#7858,.F.);
#10235=ORIENTED_EDGE('',*,*,#7859,.T.);
#10236=ORIENTED_EDGE('',*,*,#7846,.T.);
#10237=ORIENTED_EDGE('',*,*,#7847,.T.);
#10238=ORIENTED_EDGE('',*,*,#7859,.F.);
#10239=ORIENTED_EDGE('',*,*,#7858,.T.);
#10240=ORIENTED_EDGE('',*,*,#7860,.F.);
#10241=ORIENTED_EDGE('',*,*,#7860,.T.);
#10242=ORIENTED_EDGE('',*,*,#7861,.T.);
#10243=ORIENTED_EDGE('',*,*,#7853,.F.);
#10244=ORIENTED_EDGE('',*,*,#7861,.F.);
#10245=ORIENTED_EDGE('',*,*,#7862,.F.);
#10246=ORIENTED_EDGE('',*,*,#7863,.F.);
#10247=ORIENTED_EDGE('',*,*,#7864,.T.);
#10248=ORIENTED_EDGE('',*,*,#7865,.F.);
#10249=ORIENTED_EDGE('',*,*,#7866,.F.);
#10250=ORIENTED_EDGE('',*,*,#7864,.F.);
#10251=ORIENTED_EDGE('',*,*,#7867,.T.);
#10252=ORIENTED_EDGE('',*,*,#7868,.T.);
#10253=ORIENTED_EDGE('',*,*,#7865,.T.);
#10254=ORIENTED_EDGE('',*,*,#7866,.T.);
#10255=ORIENTED_EDGE('',*,*,#7868,.F.);
#10256=ORIENTED_EDGE('',*,*,#7869,.F.);
#10257=ORIENTED_EDGE('',*,*,#7870,.T.);
#10258=ORIENTED_EDGE('',*,*,#7871,.F.);
#10259=ORIENTED_EDGE('',*,*,#7872,.T.);
#10260=ORIENTED_EDGE('',*,*,#7869,.T.);
#10261=ORIENTED_EDGE('',*,*,#7872,.F.);
#10262=ORIENTED_EDGE('',*,*,#7873,.F.);
#10263=ORIENTED_EDGE('',*,*,#7874,.T.);
#10264=ORIENTED_EDGE('',*,*,#7871,.T.);
#10265=ORIENTED_EDGE('',*,*,#7874,.F.);
#10266=ORIENTED_EDGE('',*,*,#7875,.F.);
#10267=ORIENTED_EDGE('',*,*,#7876,.T.);
#10268=ORIENTED_EDGE('',*,*,#7873,.T.);
#10269=ORIENTED_EDGE('',*,*,#7876,.F.);
#10270=ORIENTED_EDGE('',*,*,#7875,.T.);
#10271=ORIENTED_EDGE('',*,*,#7867,.F.);
#10272=ORIENTED_EDGE('',*,*,#7862,.T.);
#10273=ORIENTED_EDGE('',*,*,#7863,.T.);
#10274=ORIENTED_EDGE('',*,*,#7877,.T.);
#10275=ORIENTED_EDGE('',*,*,#7870,.F.);
#10276=ORIENTED_EDGE('',*,*,#7877,.F.);
#10277=ORIENTED_EDGE('',*,*,#7878,.T.);
#10278=ORIENTED_EDGE('',*,*,#7878,.F.);
#10279=ORIENTED_EDGE('',*,*,#7879,.T.);
#10280=ORIENTED_EDGE('',*,*,#7879,.F.);
#10281=ORIENTED_EDGE('',*,*,#7880,.T.);
#10282=ORIENTED_EDGE('',*,*,#7880,.F.);
#10283=ORIENTED_EDGE('',*,*,#7881,.T.);
#10284=ORIENTED_EDGE('',*,*,#7881,.F.);
#10285=ORIENTED_EDGE('',*,*,#7882,.T.);
#10286=ORIENTED_EDGE('',*,*,#7882,.F.);
#10287=ORIENTED_EDGE('',*,*,#7883,.T.);
#10288=ORIENTED_EDGE('',*,*,#7883,.F.);
#10289=ORIENTED_EDGE('',*,*,#7884,.T.);
#10290=ORIENTED_EDGE('',*,*,#7884,.F.);
#10291=ORIENTED_EDGE('',*,*,#7885,.F.);
#10292=ORIENTED_EDGE('',*,*,#7886,.F.);
#10293=ORIENTED_EDGE('',*,*,#7887,.F.);
#10294=ORIENTED_EDGE('',*,*,#7888,.F.);
#10295=ORIENTED_EDGE('',*,*,#7887,.T.);
#10296=ORIENTED_EDGE('',*,*,#7889,.F.);
#10297=ORIENTED_EDGE('',*,*,#7890,.T.);
#10298=ORIENTED_EDGE('',*,*,#7891,.F.);
#10299=ORIENTED_EDGE('',*,*,#7892,.T.);
#10300=ORIENTED_EDGE('',*,*,#7893,.F.);
#10301=ORIENTED_EDGE('',*,*,#7894,.T.);
#10302=ORIENTED_EDGE('',*,*,#7895,.F.);
#10303=ORIENTED_EDGE('',*,*,#7894,.F.);
#10304=ORIENTED_EDGE('',*,*,#7896,.F.);
#10305=ORIENTED_EDGE('',*,*,#7897,.T.);
#10306=ORIENTED_EDGE('',*,*,#7898,.F.);
#10307=ORIENTED_EDGE('',*,*,#7899,.T.);
#10308=ORIENTED_EDGE('',*,*,#7900,.F.);
#10309=ORIENTED_EDGE('',*,*,#7901,.T.);
#10310=ORIENTED_EDGE('',*,*,#7902,.F.);
#10311=ORIENTED_EDGE('',*,*,#7903,.T.);
#10312=ORIENTED_EDGE('',*,*,#7904,.F.);
#10313=ORIENTED_EDGE('',*,*,#7886,.T.);
#10314=ORIENTED_EDGE('',*,*,#7905,.T.);
#10315=ORIENTED_EDGE('',*,*,#7906,.T.);
#10316=ORIENTED_EDGE('',*,*,#7889,.T.);
#10317=ORIENTED_EDGE('',*,*,#7907,.F.);
#10318=ORIENTED_EDGE('',*,*,#7908,.F.);
#10319=ORIENTED_EDGE('',*,*,#7890,.F.);
#10320=ORIENTED_EDGE('',*,*,#7906,.F.);
#10321=ORIENTED_EDGE('',*,*,#7908,.T.);
#10322=ORIENTED_EDGE('',*,*,#7909,.T.);
#10323=ORIENTED_EDGE('',*,*,#7910,.T.);
#10324=ORIENTED_EDGE('',*,*,#7891,.T.);
#10325=ORIENTED_EDGE('',*,*,#7911,.F.);
#10326=ORIENTED_EDGE('',*,*,#7912,.F.);
#10327=ORIENTED_EDGE('',*,*,#7892,.F.);
#10328=ORIENTED_EDGE('',*,*,#7910,.F.);
#10329=ORIENTED_EDGE('',*,*,#7912,.T.);
#10330=ORIENTED_EDGE('',*,*,#7913,.T.);
#10331=ORIENTED_EDGE('',*,*,#7914,.T.);
#10332=ORIENTED_EDGE('',*,*,#7915,.T.);
#10333=ORIENTED_EDGE('',*,*,#7896,.T.);
#10334=ORIENTED_EDGE('',*,*,#7893,.T.);
#10335=ORIENTED_EDGE('',*,*,#7916,.F.);
#10336=ORIENTED_EDGE('',*,*,#7917,.F.);
#10337=ORIENTED_EDGE('',*,*,#7897,.F.);
#10338=ORIENTED_EDGE('',*,*,#7915,.F.);
#10339=ORIENTED_EDGE('',*,*,#7917,.T.);
#10340=ORIENTED_EDGE('',*,*,#7918,.T.);
#10341=ORIENTED_EDGE('',*,*,#7919,.T.);
#10342=ORIENTED_EDGE('',*,*,#7898,.T.);
#10343=ORIENTED_EDGE('',*,*,#7920,.F.);
#10344=ORIENTED_EDGE('',*,*,#7921,.F.);
#10345=ORIENTED_EDGE('',*,*,#7899,.F.);
#10346=ORIENTED_EDGE('',*,*,#7919,.F.);
#10347=ORIENTED_EDGE('',*,*,#7921,.T.);
#10348=ORIENTED_EDGE('',*,*,#7922,.T.);
#10349=ORIENTED_EDGE('',*,*,#7923,.T.);
#10350=ORIENTED_EDGE('',*,*,#7900,.T.);
#10351=ORIENTED_EDGE('',*,*,#7901,.F.);
#10352=ORIENTED_EDGE('',*,*,#7923,.F.);
#10353=ORIENTED_EDGE('',*,*,#7924,.F.);
#10354=ORIENTED_EDGE('',*,*,#7925,.F.);
#10355=ORIENTED_EDGE('',*,*,#7926,.F.);
#10356=ORIENTED_EDGE('',*,*,#7927,.T.);
#10357=ORIENTED_EDGE('',*,*,#7913,.F.);
#10358=ORIENTED_EDGE('',*,*,#7911,.T.);
#10359=ORIENTED_EDGE('',*,*,#7909,.F.);
#10360=ORIENTED_EDGE('',*,*,#7907,.T.);
#10361=ORIENTED_EDGE('',*,*,#7905,.F.);
#10362=ORIENTED_EDGE('',*,*,#7885,.T.);
#10363=ORIENTED_EDGE('',*,*,#7928,.F.);
#10364=ORIENTED_EDGE('',*,*,#7929,.T.);
#10365=ORIENTED_EDGE('',*,*,#7930,.F.);
#10366=ORIENTED_EDGE('',*,*,#7924,.T.);
#10367=ORIENTED_EDGE('',*,*,#7922,.F.);
#10368=ORIENTED_EDGE('',*,*,#7920,.T.);
#10369=ORIENTED_EDGE('',*,*,#7918,.F.);
#10370=ORIENTED_EDGE('',*,*,#7916,.T.);
#10371=ORIENTED_EDGE('',*,*,#7914,.F.);
#10372=ORIENTED_EDGE('',*,*,#7927,.F.);
#10373=ORIENTED_EDGE('',*,*,#7888,.T.);
#10374=ORIENTED_EDGE('',*,*,#7904,.T.);
#10375=ORIENTED_EDGE('',*,*,#7931,.T.);
#10376=ORIENTED_EDGE('',*,*,#7928,.T.);
#10377=ORIENTED_EDGE('',*,*,#7903,.F.);
#10378=ORIENTED_EDGE('',*,*,#7932,.F.);
#10379=ORIENTED_EDGE('',*,*,#7929,.F.);
#10380=ORIENTED_EDGE('',*,*,#7931,.F.);
#10381=ORIENTED_EDGE('',*,*,#7895,.T.);
#10382=ORIENTED_EDGE('',*,*,#7926,.T.);
#10383=ORIENTED_EDGE('',*,*,#7925,.T.);
#10384=ORIENTED_EDGE('',*,*,#7930,.T.);
#10385=ORIENTED_EDGE('',*,*,#7932,.T.);
#10386=ORIENTED_EDGE('',*,*,#7902,.T.);
#10387=ORIENTED_EDGE('',*,*,#7933,.F.);
#10388=ORIENTED_EDGE('',*,*,#7934,.T.);
#10389=ORIENTED_EDGE('',*,*,#7935,.F.);
#10390=ORIENTED_EDGE('',*,*,#7936,.T.);
#10391=ORIENTED_EDGE('',*,*,#7933,.T.);
#10392=ORIENTED_EDGE('',*,*,#7936,.F.);
#10393=ORIENTED_EDGE('',*,*,#7935,.T.);
#10394=ORIENTED_EDGE('',*,*,#7937,.F.);
#10395=ORIENTED_EDGE('',*,*,#7937,.T.);
#10396=ORIENTED_EDGE('',*,*,#7938,.T.);
#10397=ORIENTED_EDGE('',*,*,#7934,.F.);
#10398=ORIENTED_EDGE('',*,*,#7938,.F.);
#10399=ORIENTED_EDGE('',*,*,#7939,.F.);
#10400=ORIENTED_EDGE('',*,*,#7940,.T.);
#10401=ORIENTED_EDGE('',*,*,#7941,.F.);
#10402=ORIENTED_EDGE('',*,*,#7942,.T.);
#10403=ORIENTED_EDGE('',*,*,#7939,.T.);
#10404=ORIENTED_EDGE('',*,*,#7942,.F.);
#10405=ORIENTED_EDGE('',*,*,#7941,.T.);
#10406=ORIENTED_EDGE('',*,*,#7943,.F.);
#10407=ORIENTED_EDGE('',*,*,#7943,.T.);
#10408=ORIENTED_EDGE('',*,*,#7944,.T.);
#10409=ORIENTED_EDGE('',*,*,#7940,.F.);
#10410=ORIENTED_EDGE('',*,*,#7944,.F.);
#10411=ORIENTED_EDGE('',*,*,#7945,.F.);
#10412=ORIENTED_EDGE('',*,*,#7946,.T.);
#10413=ORIENTED_EDGE('',*,*,#7947,.F.);
#10414=ORIENTED_EDGE('',*,*,#7946,.F.);
#10415=ORIENTED_EDGE('',*,*,#7948,.F.);
#10416=ORIENTED_EDGE('',*,*,#7949,.T.);
#10417=ORIENTED_EDGE('',*,*,#7950,.F.);
#10418=ORIENTED_EDGE('',*,*,#7949,.F.);
#10419=ORIENTED_EDGE('',*,*,#7951,.F.);
#10420=ORIENTED_EDGE('',*,*,#7952,.T.);
#10421=ORIENTED_EDGE('',*,*,#7953,.F.);
#10422=ORIENTED_EDGE('',*,*,#7952,.F.);
#10423=ORIENTED_EDGE('',*,*,#7954,.F.);
#10424=ORIENTED_EDGE('',*,*,#7955,.T.);
#10425=ORIENTED_EDGE('',*,*,#7956,.F.);
#10426=ORIENTED_EDGE('',*,*,#7955,.F.);
#10427=ORIENTED_EDGE('',*,*,#7957,.F.);
#10428=ORIENTED_EDGE('',*,*,#7958,.T.);
#10429=ORIENTED_EDGE('',*,*,#7959,.F.);
#10430=ORIENTED_EDGE('',*,*,#7958,.F.);
#10431=ORIENTED_EDGE('',*,*,#7960,.F.);
#10432=ORIENTED_EDGE('',*,*,#7961,.T.);
#10433=ORIENTED_EDGE('',*,*,#7962,.F.);
#10434=ORIENTED_EDGE('',*,*,#7961,.F.);
#10435=ORIENTED_EDGE('',*,*,#7963,.F.);
#10436=ORIENTED_EDGE('',*,*,#7964,.T.);
#10437=ORIENTED_EDGE('',*,*,#7965,.F.);
#10438=ORIENTED_EDGE('',*,*,#7964,.F.);
#10439=ORIENTED_EDGE('',*,*,#7966,.F.);
#10440=ORIENTED_EDGE('',*,*,#7967,.T.);
#10441=ORIENTED_EDGE('',*,*,#7968,.F.);
#10442=ORIENTED_EDGE('',*,*,#7967,.F.);
#10443=ORIENTED_EDGE('',*,*,#7969,.F.);
#10444=ORIENTED_EDGE('',*,*,#7970,.F.);
#10445=ORIENTED_EDGE('',*,*,#7971,.T.);
#10446=ORIENTED_EDGE('',*,*,#7972,.F.);
#10447=ORIENTED_EDGE('',*,*,#7973,.F.);
#10448=ORIENTED_EDGE('',*,*,#7974,.F.);
#10449=ORIENTED_EDGE('',*,*,#7975,.F.);
#10450=ORIENTED_EDGE('',*,*,#7976,.F.);
#10451=ORIENTED_EDGE('',*,*,#7977,.F.);
#10452=ORIENTED_EDGE('',*,*,#7975,.T.);
#10453=ORIENTED_EDGE('',*,*,#7978,.F.);
#10454=ORIENTED_EDGE('',*,*,#7971,.F.);
#10455=ORIENTED_EDGE('',*,*,#7969,.T.);
#10456=ORIENTED_EDGE('',*,*,#7979,.F.);
#10457=ORIENTED_EDGE('',*,*,#7980,.F.);
#10458=ORIENTED_EDGE('',*,*,#7981,.T.);
#10459=ORIENTED_EDGE('',*,*,#7973,.T.);
#10460=ORIENTED_EDGE('',*,*,#7982,.T.);
#10461=ORIENTED_EDGE('',*,*,#7983,.F.);
#10462=ORIENTED_EDGE('',*,*,#7984,.F.);
#10463=ORIENTED_EDGE('',*,*,#7981,.F.);
#10464=ORIENTED_EDGE('',*,*,#7985,.F.);
#10465=ORIENTED_EDGE('',*,*,#7986,.T.);
#10466=ORIENTED_EDGE('',*,*,#7987,.T.);
#10467=ORIENTED_EDGE('',*,*,#7988,.T.);
#10468=ORIENTED_EDGE('',*,*,#7989,.F.);
#10469=ORIENTED_EDGE('',*,*,#7990,.F.);
#10470=ORIENTED_EDGE('',*,*,#7982,.F.);
#10471=ORIENTED_EDGE('',*,*,#7976,.T.);
#10472=ORIENTED_EDGE('',*,*,#7977,.T.);
#10473=ORIENTED_EDGE('',*,*,#7970,.T.);
#10474=ORIENTED_EDGE('',*,*,#7966,.T.);
#10475=ORIENTED_EDGE('',*,*,#7963,.T.);
#10476=ORIENTED_EDGE('',*,*,#7960,.T.);
#10477=ORIENTED_EDGE('',*,*,#7957,.T.);
#10478=ORIENTED_EDGE('',*,*,#7954,.T.);
#10479=ORIENTED_EDGE('',*,*,#7951,.T.);
#10480=ORIENTED_EDGE('',*,*,#7948,.T.);
#10481=ORIENTED_EDGE('',*,*,#7945,.T.);
#10482=ORIENTED_EDGE('',*,*,#7991,.F.);
#10483=ORIENTED_EDGE('',*,*,#7988,.F.);
#10484=ORIENTED_EDGE('',*,*,#7992,.T.);
#10485=ORIENTED_EDGE('',*,*,#7993,.F.);
#10486=ORIENTED_EDGE('',*,*,#7994,.F.);
#10487=ORIENTED_EDGE('',*,*,#7995,.F.);
#10488=ORIENTED_EDGE('',*,*,#7996,.F.);
#10489=ORIENTED_EDGE('',*,*,#7986,.F.);
#10490=ORIENTED_EDGE('',*,*,#7987,.F.);
#10491=ORIENTED_EDGE('',*,*,#7996,.T.);
#10492=ORIENTED_EDGE('',*,*,#7997,.F.);
#10493=ORIENTED_EDGE('',*,*,#7992,.F.);
#10494=ORIENTED_EDGE('',*,*,#7994,.T.);
#10495=ORIENTED_EDGE('',*,*,#7985,.T.);
#10496=ORIENTED_EDGE('',*,*,#7980,.T.);
#10497=ORIENTED_EDGE('',*,*,#7998,.F.);
#10498=ORIENTED_EDGE('',*,*,#7991,.T.);
#10499=ORIENTED_EDGE('',*,*,#7999,.F.);
#10500=ORIENTED_EDGE('',*,*,#8000,.F.);
#10501=ORIENTED_EDGE('',*,*,#7989,.T.);
#10502=ORIENTED_EDGE('',*,*,#7983,.T.);
#10503=ORIENTED_EDGE('',*,*,#7990,.T.);
#10504=ORIENTED_EDGE('',*,*,#8000,.T.);
#10505=ORIENTED_EDGE('',*,*,#8001,.F.);
#10506=ORIENTED_EDGE('',*,*,#7984,.T.);
#10507=ORIENTED_EDGE('',*,*,#8001,.T.);
#10508=ORIENTED_EDGE('',*,*,#7999,.T.);
#10509=ORIENTED_EDGE('',*,*,#7993,.T.);
#10510=ORIENTED_EDGE('',*,*,#7997,.T.);
#10511=ORIENTED_EDGE('',*,*,#7995,.T.);
#10512=ORIENTED_EDGE('',*,*,#7998,.T.);
#10513=ORIENTED_EDGE('',*,*,#7979,.T.);
#10514=ORIENTED_EDGE('',*,*,#7972,.T.);
#10515=ORIENTED_EDGE('',*,*,#7978,.T.);
#10516=ORIENTED_EDGE('',*,*,#7974,.T.);
#10517=ORIENTED_EDGE('',*,*,#7968,.T.);
#10518=ORIENTED_EDGE('',*,*,#7965,.T.);
#10519=ORIENTED_EDGE('',*,*,#7962,.T.);
#10520=ORIENTED_EDGE('',*,*,#7959,.T.);
#10521=ORIENTED_EDGE('',*,*,#7956,.T.);
#10522=ORIENTED_EDGE('',*,*,#7953,.T.);
#10523=ORIENTED_EDGE('',*,*,#7950,.T.);
#10524=ORIENTED_EDGE('',*,*,#7947,.T.);
#10525=ORIENTED_EDGE('',*,*,#8002,.T.);
#10526=ORIENTED_EDGE('',*,*,#8003,.T.);
#10527=ORIENTED_EDGE('',*,*,#8004,.F.);
#10528=ORIENTED_EDGE('',*,*,#8005,.F.);
#10529=ORIENTED_EDGE('',*,*,#8006,.T.);
#10530=ORIENTED_EDGE('',*,*,#8005,.T.);
#10531=ORIENTED_EDGE('',*,*,#8007,.F.);
#10532=ORIENTED_EDGE('',*,*,#8008,.F.);
#10533=ORIENTED_EDGE('',*,*,#8009,.T.);
#10534=ORIENTED_EDGE('',*,*,#8008,.T.);
#10535=ORIENTED_EDGE('',*,*,#8010,.F.);
#10536=ORIENTED_EDGE('',*,*,#8011,.F.);
#10537=ORIENTED_EDGE('',*,*,#8012,.T.);
#10538=ORIENTED_EDGE('',*,*,#8011,.T.);
#10539=ORIENTED_EDGE('',*,*,#8013,.F.);
#10540=ORIENTED_EDGE('',*,*,#8003,.F.);
#10541=ORIENTED_EDGE('',*,*,#8013,.T.);
#10542=ORIENTED_EDGE('',*,*,#8010,.T.);
#10543=ORIENTED_EDGE('',*,*,#8007,.T.);
#10544=ORIENTED_EDGE('',*,*,#8004,.T.);
#10545=ORIENTED_EDGE('',*,*,#8012,.F.);
#10546=ORIENTED_EDGE('',*,*,#8002,.F.);
#10547=ORIENTED_EDGE('',*,*,#8006,.F.);
#10548=ORIENTED_EDGE('',*,*,#8009,.F.);
#10549=ORIENTED_EDGE('',*,*,#8014,.T.);
#10550=ORIENTED_EDGE('',*,*,#8015,.T.);
#10551=ORIENTED_EDGE('',*,*,#8016,.F.);
#10552=ORIENTED_EDGE('',*,*,#8017,.F.);
#10553=ORIENTED_EDGE('',*,*,#8018,.T.);
#10554=ORIENTED_EDGE('',*,*,#8017,.T.);
#10555=ORIENTED_EDGE('',*,*,#8019,.F.);
#10556=ORIENTED_EDGE('',*,*,#8020,.F.);
#10557=ORIENTED_EDGE('',*,*,#8021,.T.);
#10558=ORIENTED_EDGE('',*,*,#8020,.T.);
#10559=ORIENTED_EDGE('',*,*,#8022,.F.);
#10560=ORIENTED_EDGE('',*,*,#8023,.F.);
#10561=ORIENTED_EDGE('',*,*,#8024,.T.);
#10562=ORIENTED_EDGE('',*,*,#8023,.T.);
#10563=ORIENTED_EDGE('',*,*,#8025,.F.);
#10564=ORIENTED_EDGE('',*,*,#8015,.F.);
#10565=ORIENTED_EDGE('',*,*,#8025,.T.);
#10566=ORIENTED_EDGE('',*,*,#8022,.T.);
#10567=ORIENTED_EDGE('',*,*,#8019,.T.);
#10568=ORIENTED_EDGE('',*,*,#8016,.T.);
#10569=ORIENTED_EDGE('',*,*,#8024,.F.);
#10570=ORIENTED_EDGE('',*,*,#8014,.F.);
#10571=ORIENTED_EDGE('',*,*,#8018,.F.);
#10572=ORIENTED_EDGE('',*,*,#8021,.F.);
#10573=ORIENTED_EDGE('',*,*,#8026,.T.);
#10574=ORIENTED_EDGE('',*,*,#8027,.T.);
#10575=ORIENTED_EDGE('',*,*,#8028,.F.);
#10576=ORIENTED_EDGE('',*,*,#8029,.F.);
#10577=ORIENTED_EDGE('',*,*,#8030,.T.);
#10578=ORIENTED_EDGE('',*,*,#8029,.T.);
#10579=ORIENTED_EDGE('',*,*,#8031,.F.);
#10580=ORIENTED_EDGE('',*,*,#8032,.F.);
#10581=ORIENTED_EDGE('',*,*,#8033,.T.);
#10582=ORIENTED_EDGE('',*,*,#8032,.T.);
#10583=ORIENTED_EDGE('',*,*,#8034,.F.);
#10584=ORIENTED_EDGE('',*,*,#8035,.F.);
#10585=ORIENTED_EDGE('',*,*,#8036,.T.);
#10586=ORIENTED_EDGE('',*,*,#8035,.T.);
#10587=ORIENTED_EDGE('',*,*,#8037,.F.);
#10588=ORIENTED_EDGE('',*,*,#8027,.F.);
#10589=ORIENTED_EDGE('',*,*,#8037,.T.);
#10590=ORIENTED_EDGE('',*,*,#8034,.T.);
#10591=ORIENTED_EDGE('',*,*,#8031,.T.);
#10592=ORIENTED_EDGE('',*,*,#8028,.T.);
#10593=ORIENTED_EDGE('',*,*,#8036,.F.);
#10594=ORIENTED_EDGE('',*,*,#8026,.F.);
#10595=ORIENTED_EDGE('',*,*,#8030,.F.);
#10596=ORIENTED_EDGE('',*,*,#8033,.F.);
#10597=ORIENTED_EDGE('',*,*,#8038,.F.);
#10598=ORIENTED_EDGE('',*,*,#8039,.T.);
#10599=ORIENTED_EDGE('',*,*,#8040,.T.);
#10600=ORIENTED_EDGE('',*,*,#8039,.F.);
#10601=ORIENTED_EDGE('',*,*,#8040,.F.);
#10602=ORIENTED_EDGE('',*,*,#8041,.F.);
#10603=ORIENTED_EDGE('',*,*,#8042,.T.);
#10604=ORIENTED_EDGE('',*,*,#8043,.F.);
#10605=ORIENTED_EDGE('',*,*,#8042,.F.);
#10606=ORIENTED_EDGE('',*,*,#8044,.F.);
#10607=ORIENTED_EDGE('',*,*,#8045,.T.);
#10608=ORIENTED_EDGE('',*,*,#8046,.F.);
#10609=ORIENTED_EDGE('',*,*,#8045,.F.);
#10610=ORIENTED_EDGE('',*,*,#8047,.F.);
#10611=ORIENTED_EDGE('',*,*,#8048,.T.);
#10612=ORIENTED_EDGE('',*,*,#8049,.F.);
#10613=ORIENTED_EDGE('',*,*,#8048,.F.);
#10614=ORIENTED_EDGE('',*,*,#8050,.T.);
#10615=ORIENTED_EDGE('',*,*,#8043,.T.);
#10616=ORIENTED_EDGE('',*,*,#8046,.T.);
#10617=ORIENTED_EDGE('',*,*,#8049,.T.);
#10618=ORIENTED_EDGE('',*,*,#8051,.F.);
#10619=ORIENTED_EDGE('',*,*,#8052,.F.);
#10620=ORIENTED_EDGE('',*,*,#8041,.T.);
#10621=ORIENTED_EDGE('',*,*,#8044,.T.);
#10622=ORIENTED_EDGE('',*,*,#8047,.T.);
#10623=ORIENTED_EDGE('',*,*,#8053,.F.);
#10624=ORIENTED_EDGE('',*,*,#8050,.F.);
#10625=ORIENTED_EDGE('',*,*,#8054,.T.);
#10626=ORIENTED_EDGE('',*,*,#8052,.T.);
#10627=ORIENTED_EDGE('',*,*,#8054,.F.);
#10628=ORIENTED_EDGE('',*,*,#8053,.T.);
#10629=ORIENTED_EDGE('',*,*,#8055,.T.);
#10630=ORIENTED_EDGE('',*,*,#8056,.T.);
#10631=ORIENTED_EDGE('',*,*,#8055,.F.);
#10632=ORIENTED_EDGE('',*,*,#8057,.F.);
#10633=ORIENTED_EDGE('',*,*,#8058,.T.);
#10634=ORIENTED_EDGE('',*,*,#8051,.T.);
#10635=ORIENTED_EDGE('',*,*,#8058,.F.);
#10636=ORIENTED_EDGE('',*,*,#8057,.T.);
#10637=ORIENTED_EDGE('',*,*,#8056,.F.);
#10638=ORIENTED_EDGE('',*,*,#8038,.T.);
#10639=ORIENTED_EDGE('',*,*,#8059,.F.);
#10640=ORIENTED_EDGE('',*,*,#8060,.T.);
#10641=ORIENTED_EDGE('',*,*,#8061,.T.);
#10642=ORIENTED_EDGE('',*,*,#8060,.F.);
#10643=ORIENTED_EDGE('',*,*,#8062,.F.);
#10644=ORIENTED_EDGE('',*,*,#8063,.T.);
#10645=ORIENTED_EDGE('',*,*,#8064,.T.);
#10646=ORIENTED_EDGE('',*,*,#8063,.F.);
#10647=ORIENTED_EDGE('',*,*,#8062,.T.);
#10648=ORIENTED_EDGE('',*,*,#8059,.T.);
#10649=ORIENTED_EDGE('',*,*,#8064,.F.);
#10650=ORIENTED_EDGE('',*,*,#8061,.F.);
#10651=ORIENTED_EDGE('',*,*,#8065,.F.);
#10652=ORIENTED_EDGE('',*,*,#8066,.T.);
#10653=ORIENTED_EDGE('',*,*,#8067,.T.);
#10654=ORIENTED_EDGE('',*,*,#8066,.F.);
#10655=ORIENTED_EDGE('',*,*,#8068,.F.);
#10656=ORIENTED_EDGE('',*,*,#8069,.T.);
#10657=ORIENTED_EDGE('',*,*,#8070,.T.);
#10658=ORIENTED_EDGE('',*,*,#8069,.F.);
#10659=ORIENTED_EDGE('',*,*,#8068,.T.);
#10660=ORIENTED_EDGE('',*,*,#8065,.T.);
#10661=ORIENTED_EDGE('',*,*,#8070,.F.);
#10662=ORIENTED_EDGE('',*,*,#8067,.F.);
#10663=ORIENTED_EDGE('',*,*,#8071,.F.);
#10664=ORIENTED_EDGE('',*,*,#8072,.T.);
#10665=ORIENTED_EDGE('',*,*,#8073,.T.);
#10666=ORIENTED_EDGE('',*,*,#8072,.F.);
#10667=ORIENTED_EDGE('',*,*,#8074,.F.);
#10668=ORIENTED_EDGE('',*,*,#8075,.T.);
#10669=ORIENTED_EDGE('',*,*,#8076,.T.);
#10670=ORIENTED_EDGE('',*,*,#8075,.F.);
#10671=ORIENTED_EDGE('',*,*,#8074,.T.);
#10672=ORIENTED_EDGE('',*,*,#8071,.T.);
#10673=ORIENTED_EDGE('',*,*,#8076,.F.);
#10674=ORIENTED_EDGE('',*,*,#8073,.F.);
#10675=ORIENTED_EDGE('',*,*,#8077,.F.);
#10676=ORIENTED_EDGE('',*,*,#8078,.T.);
#10677=ORIENTED_EDGE('',*,*,#8079,.T.);
#10678=ORIENTED_EDGE('',*,*,#8078,.F.);
#10679=ORIENTED_EDGE('',*,*,#8080,.F.);
#10680=ORIENTED_EDGE('',*,*,#8081,.T.);
#10681=ORIENTED_EDGE('',*,*,#8082,.T.);
#10682=ORIENTED_EDGE('',*,*,#8081,.F.);
#10683=ORIENTED_EDGE('',*,*,#8080,.T.);
#10684=ORIENTED_EDGE('',*,*,#8077,.T.);
#10685=ORIENTED_EDGE('',*,*,#8082,.F.);
#10686=ORIENTED_EDGE('',*,*,#8079,.F.);
#10687=ORIENTED_EDGE('',*,*,#8083,.F.);
#10688=ORIENTED_EDGE('',*,*,#8084,.T.);
#10689=ORIENTED_EDGE('',*,*,#8085,.T.);
#10690=ORIENTED_EDGE('',*,*,#8084,.F.);
#10691=ORIENTED_EDGE('',*,*,#8085,.F.);
#10692=ORIENTED_EDGE('',*,*,#8086,.F.);
#10693=ORIENTED_EDGE('',*,*,#8087,.T.);
#10694=ORIENTED_EDGE('',*,*,#8088,.F.);
#10695=ORIENTED_EDGE('',*,*,#8087,.F.);
#10696=ORIENTED_EDGE('',*,*,#8089,.F.);
#10697=ORIENTED_EDGE('',*,*,#8090,.T.);
#10698=ORIENTED_EDGE('',*,*,#8091,.F.);
#10699=ORIENTED_EDGE('',*,*,#8090,.F.);
#10700=ORIENTED_EDGE('',*,*,#8092,.F.);
#10701=ORIENTED_EDGE('',*,*,#8093,.T.);
#10702=ORIENTED_EDGE('',*,*,#8094,.F.);
#10703=ORIENTED_EDGE('',*,*,#8093,.F.);
#10704=ORIENTED_EDGE('',*,*,#8095,.T.);
#10705=ORIENTED_EDGE('',*,*,#8088,.T.);
#10706=ORIENTED_EDGE('',*,*,#8091,.T.);
#10707=ORIENTED_EDGE('',*,*,#8094,.T.);
#10708=ORIENTED_EDGE('',*,*,#8096,.F.);
#10709=ORIENTED_EDGE('',*,*,#8097,.F.);
#10710=ORIENTED_EDGE('',*,*,#8086,.T.);
#10711=ORIENTED_EDGE('',*,*,#8089,.T.);
#10712=ORIENTED_EDGE('',*,*,#8092,.T.);
#10713=ORIENTED_EDGE('',*,*,#8098,.F.);
#10714=ORIENTED_EDGE('',*,*,#8095,.F.);
#10715=ORIENTED_EDGE('',*,*,#8099,.T.);
#10716=ORIENTED_EDGE('',*,*,#8097,.T.);
#10717=ORIENTED_EDGE('',*,*,#8099,.F.);
#10718=ORIENTED_EDGE('',*,*,#8098,.T.);
#10719=ORIENTED_EDGE('',*,*,#8100,.T.);
#10720=ORIENTED_EDGE('',*,*,#8101,.T.);
#10721=ORIENTED_EDGE('',*,*,#8100,.F.);
#10722=ORIENTED_EDGE('',*,*,#8102,.F.);
#10723=ORIENTED_EDGE('',*,*,#8103,.T.);
#10724=ORIENTED_EDGE('',*,*,#8096,.T.);
#10725=ORIENTED_EDGE('',*,*,#8103,.F.);
#10726=ORIENTED_EDGE('',*,*,#8102,.T.);
#10727=ORIENTED_EDGE('',*,*,#8101,.F.);
#10728=ORIENTED_EDGE('',*,*,#8083,.T.);
#10729=ORIENTED_EDGE('',*,*,#8104,.F.);
#10730=ORIENTED_EDGE('',*,*,#8105,.T.);
#10731=ORIENTED_EDGE('',*,*,#8106,.T.);
#10732=ORIENTED_EDGE('',*,*,#8105,.F.);
#10733=ORIENTED_EDGE('',*,*,#8107,.F.);
#10734=ORIENTED_EDGE('',*,*,#8108,.T.);
#10735=ORIENTED_EDGE('',*,*,#8109,.T.);
#10736=ORIENTED_EDGE('',*,*,#8108,.F.);
#10737=ORIENTED_EDGE('',*,*,#8107,.T.);
#10738=ORIENTED_EDGE('',*,*,#8104,.T.);
#10739=ORIENTED_EDGE('',*,*,#8109,.F.);
#10740=ORIENTED_EDGE('',*,*,#8106,.F.);
#10741=ORIENTED_EDGE('',*,*,#8110,.F.);
#10742=ORIENTED_EDGE('',*,*,#8111,.T.);
#10743=ORIENTED_EDGE('',*,*,#8112,.T.);
#10744=ORIENTED_EDGE('',*,*,#8111,.F.);
#10745=ORIENTED_EDGE('',*,*,#8113,.F.);
#10746=ORIENTED_EDGE('',*,*,#8114,.T.);
#10747=ORIENTED_EDGE('',*,*,#8115,.T.);
#10748=ORIENTED_EDGE('',*,*,#8114,.F.);
#10749=ORIENTED_EDGE('',*,*,#8113,.T.);
#10750=ORIENTED_EDGE('',*,*,#8110,.T.);
#10751=ORIENTED_EDGE('',*,*,#8115,.F.);
#10752=ORIENTED_EDGE('',*,*,#8112,.F.);
#10753=ORIENTED_EDGE('',*,*,#8116,.F.);
#10754=ORIENTED_EDGE('',*,*,#8117,.T.);
#10755=ORIENTED_EDGE('',*,*,#8118,.T.);
#10756=ORIENTED_EDGE('',*,*,#8117,.F.);
#10757=ORIENTED_EDGE('',*,*,#8119,.F.);
#10758=ORIENTED_EDGE('',*,*,#8120,.T.);
#10759=ORIENTED_EDGE('',*,*,#8121,.T.);
#10760=ORIENTED_EDGE('',*,*,#8120,.F.);
#10761=ORIENTED_EDGE('',*,*,#8119,.T.);
#10762=ORIENTED_EDGE('',*,*,#8116,.T.);
#10763=ORIENTED_EDGE('',*,*,#8121,.F.);
#10764=ORIENTED_EDGE('',*,*,#8118,.F.);
#10765=ORIENTED_EDGE('',*,*,#8122,.F.);
#10766=ORIENTED_EDGE('',*,*,#8123,.F.);
#10767=ORIENTED_EDGE('',*,*,#8124,.T.);
#10768=ORIENTED_EDGE('',*,*,#8122,.T.);
#10769=ORIENTED_EDGE('',*,*,#8124,.F.);
#10770=ORIENTED_EDGE('',*,*,#8125,.F.);
#10771=ORIENTED_EDGE('',*,*,#8126,.T.);
#10772=ORIENTED_EDGE('',*,*,#8123,.T.);
#10773=ORIENTED_EDGE('',*,*,#8126,.F.);
#10774=ORIENTED_EDGE('',*,*,#8127,.F.);
#10775=ORIENTED_EDGE('',*,*,#8128,.T.);
#10776=ORIENTED_EDGE('',*,*,#8125,.T.);
#10777=ORIENTED_EDGE('',*,*,#8128,.F.);
#10778=ORIENTED_EDGE('',*,*,#8127,.T.);
#10779=ORIENTED_EDGE('',*,*,#8129,.F.);
#10780=ORIENTED_EDGE('',*,*,#8130,.F.);
#10781=ORIENTED_EDGE('',*,*,#8131,.T.);
#10782=ORIENTED_EDGE('',*,*,#8129,.T.);
#10783=ORIENTED_EDGE('',*,*,#8131,.F.);
#10784=ORIENTED_EDGE('',*,*,#8132,.F.);
#10785=ORIENTED_EDGE('',*,*,#8133,.T.);
#10786=ORIENTED_EDGE('',*,*,#8130,.T.);
#10787=ORIENTED_EDGE('',*,*,#8133,.F.);
#10788=ORIENTED_EDGE('',*,*,#8134,.F.);
#10789=ORIENTED_EDGE('',*,*,#8135,.T.);
#10790=ORIENTED_EDGE('',*,*,#8132,.T.);
#10791=ORIENTED_EDGE('',*,*,#8135,.F.);
#10792=ORIENTED_EDGE('',*,*,#8134,.T.);
#10793=ORIENTED_EDGE('',*,*,#8136,.T.);
#10794=ORIENTED_EDGE('',*,*,#8137,.T.);
#10795=ORIENTED_EDGE('',*,*,#8138,.T.);
#10796=ORIENTED_EDGE('',*,*,#8139,.F.);
#10797=ORIENTED_EDGE('',*,*,#8140,.T.);
#10798=ORIENTED_EDGE('',*,*,#8141,.T.);
#10799=ORIENTED_EDGE('',*,*,#8142,.T.);
#10800=ORIENTED_EDGE('',*,*,#8137,.F.);
#10801=ORIENTED_EDGE('',*,*,#8143,.T.);
#10802=ORIENTED_EDGE('',*,*,#8144,.T.);
#10803=ORIENTED_EDGE('',*,*,#8145,.T.);
#10804=ORIENTED_EDGE('',*,*,#8141,.F.);
#10805=ORIENTED_EDGE('',*,*,#8146,.T.);
#10806=ORIENTED_EDGE('',*,*,#8147,.T.);
#10807=ORIENTED_EDGE('',*,*,#8148,.T.);
#10808=ORIENTED_EDGE('',*,*,#8144,.F.);
#10809=ORIENTED_EDGE('',*,*,#8149,.T.);
#10810=ORIENTED_EDGE('',*,*,#8150,.T.);
#10811=ORIENTED_EDGE('',*,*,#8151,.T.);
#10812=ORIENTED_EDGE('',*,*,#8147,.F.);
#10813=ORIENTED_EDGE('',*,*,#8152,.T.);
#10814=ORIENTED_EDGE('',*,*,#8139,.T.);
#10815=ORIENTED_EDGE('',*,*,#8153,.T.);
#10816=ORIENTED_EDGE('',*,*,#8150,.F.);
#10817=ORIENTED_EDGE('',*,*,#8152,.F.);
#10818=ORIENTED_EDGE('',*,*,#8149,.F.);
#10819=ORIENTED_EDGE('',*,*,#8146,.F.);
#10820=ORIENTED_EDGE('',*,*,#8143,.F.);
#10821=ORIENTED_EDGE('',*,*,#8140,.F.);
#10822=ORIENTED_EDGE('',*,*,#8136,.F.);
#10823=ORIENTED_EDGE('',*,*,#8153,.F.);
#10824=ORIENTED_EDGE('',*,*,#8138,.F.);
#10825=ORIENTED_EDGE('',*,*,#8142,.F.);
#10826=ORIENTED_EDGE('',*,*,#8145,.F.);
#10827=ORIENTED_EDGE('',*,*,#8148,.F.);
#10828=ORIENTED_EDGE('',*,*,#8151,.F.);
#10829=ORIENTED_EDGE('',*,*,#8154,.F.);
#10830=ORIENTED_EDGE('',*,*,#8155,.T.);
#10831=ORIENTED_EDGE('',*,*,#8156,.F.);
#10832=ORIENTED_EDGE('',*,*,#8155,.F.);
#10833=ORIENTED_EDGE('',*,*,#8157,.F.);
#10834=ORIENTED_EDGE('',*,*,#8158,.T.);
#10835=ORIENTED_EDGE('',*,*,#8159,.F.);
#10836=ORIENTED_EDGE('',*,*,#8158,.F.);
#10837=ORIENTED_EDGE('',*,*,#8160,.F.);
#10838=ORIENTED_EDGE('',*,*,#8161,.T.);
#10839=ORIENTED_EDGE('',*,*,#8162,.F.);
#10840=ORIENTED_EDGE('',*,*,#8161,.F.);
#10841=ORIENTED_EDGE('',*,*,#8163,.T.);
#10842=ORIENTED_EDGE('',*,*,#8164,.T.);
#10843=ORIENTED_EDGE('',*,*,#8165,.F.);
#10844=ORIENTED_EDGE('',*,*,#8166,.F.);
#10845=ORIENTED_EDGE('',*,*,#8167,.T.);
#10846=ORIENTED_EDGE('',*,*,#8166,.T.);
#10847=ORIENTED_EDGE('',*,*,#8168,.F.);
#10848=ORIENTED_EDGE('',*,*,#8169,.F.);
#10849=ORIENTED_EDGE('',*,*,#8156,.T.);
#10850=ORIENTED_EDGE('',*,*,#8159,.T.);
#10851=ORIENTED_EDGE('',*,*,#8162,.T.);
#10852=ORIENTED_EDGE('',*,*,#8170,.T.);
#10853=ORIENTED_EDGE('',*,*,#8169,.T.);
#10854=ORIENTED_EDGE('',*,*,#8171,.F.);
#10855=ORIENTED_EDGE('',*,*,#8172,.F.);
#10856=ORIENTED_EDGE('',*,*,#8173,.T.);
#10857=ORIENTED_EDGE('',*,*,#8172,.T.);
#10858=ORIENTED_EDGE('',*,*,#8174,.F.);
#10859=ORIENTED_EDGE('',*,*,#8164,.F.);
#10860=ORIENTED_EDGE('',*,*,#8154,.T.);
#10861=ORIENTED_EDGE('',*,*,#8157,.T.);
#10862=ORIENTED_EDGE('',*,*,#8160,.T.);
#10863=ORIENTED_EDGE('',*,*,#8174,.T.);
#10864=ORIENTED_EDGE('',*,*,#8171,.T.);
#10865=ORIENTED_EDGE('',*,*,#8168,.T.);
#10866=ORIENTED_EDGE('',*,*,#8165,.T.);
#10867=ORIENTED_EDGE('',*,*,#8173,.F.);
#10868=ORIENTED_EDGE('',*,*,#8163,.F.);
#10869=ORIENTED_EDGE('',*,*,#8167,.F.);
#10870=ORIENTED_EDGE('',*,*,#8170,.F.);
#10871=ORIENTED_EDGE('',*,*,#8175,.F.);
#10872=ORIENTED_EDGE('',*,*,#8176,.T.);
#10873=ORIENTED_EDGE('',*,*,#8177,.F.);
#10874=ORIENTED_EDGE('',*,*,#8176,.F.);
#10875=ORIENTED_EDGE('',*,*,#8178,.F.);
#10876=ORIENTED_EDGE('',*,*,#8179,.T.);
#10877=ORIENTED_EDGE('',*,*,#8180,.F.);
#10878=ORIENTED_EDGE('',*,*,#8179,.F.);
#10879=ORIENTED_EDGE('',*,*,#8181,.F.);
#10880=ORIENTED_EDGE('',*,*,#8182,.T.);
#10881=ORIENTED_EDGE('',*,*,#8183,.F.);
#10882=ORIENTED_EDGE('',*,*,#8182,.F.);
#10883=ORIENTED_EDGE('',*,*,#8184,.T.);
#10884=ORIENTED_EDGE('',*,*,#8185,.T.);
#10885=ORIENTED_EDGE('',*,*,#8186,.F.);
#10886=ORIENTED_EDGE('',*,*,#8187,.F.);
#10887=ORIENTED_EDGE('',*,*,#8188,.T.);
#10888=ORIENTED_EDGE('',*,*,#8187,.T.);
#10889=ORIENTED_EDGE('',*,*,#8189,.F.);
#10890=ORIENTED_EDGE('',*,*,#8190,.F.);
#10891=ORIENTED_EDGE('',*,*,#8191,.T.);
#10892=ORIENTED_EDGE('',*,*,#8190,.T.);
#10893=ORIENTED_EDGE('',*,*,#8192,.F.);
#10894=ORIENTED_EDGE('',*,*,#8193,.F.);
#10895=ORIENTED_EDGE('',*,*,#8194,.T.);
#10896=ORIENTED_EDGE('',*,*,#8193,.T.);
#10897=ORIENTED_EDGE('',*,*,#8195,.F.);
#10898=ORIENTED_EDGE('',*,*,#8185,.F.);
#10899=ORIENTED_EDGE('',*,*,#8195,.T.);
#10900=ORIENTED_EDGE('',*,*,#8192,.T.);
#10901=ORIENTED_EDGE('',*,*,#8189,.T.);
#10902=ORIENTED_EDGE('',*,*,#8186,.T.);
#10903=ORIENTED_EDGE('',*,*,#8177,.T.);
#10904=ORIENTED_EDGE('',*,*,#8180,.T.);
#10905=ORIENTED_EDGE('',*,*,#8183,.T.);
#10906=ORIENTED_EDGE('',*,*,#8194,.F.);
#10907=ORIENTED_EDGE('',*,*,#8184,.F.);
#10908=ORIENTED_EDGE('',*,*,#8188,.F.);
#10909=ORIENTED_EDGE('',*,*,#8191,.F.);
#10910=ORIENTED_EDGE('',*,*,#8175,.T.);
#10911=ORIENTED_EDGE('',*,*,#8178,.T.);
#10912=ORIENTED_EDGE('',*,*,#8181,.T.);
#10913=ORIENTED_EDGE('',*,*,#8196,.F.);
#10914=ORIENTED_EDGE('',*,*,#8197,.T.);
#10915=ORIENTED_EDGE('',*,*,#8198,.F.);
#10916=ORIENTED_EDGE('',*,*,#8197,.F.);
#10917=ORIENTED_EDGE('',*,*,#8199,.F.);
#10918=ORIENTED_EDGE('',*,*,#8200,.T.);
#10919=ORIENTED_EDGE('',*,*,#8201,.F.);
#10920=ORIENTED_EDGE('',*,*,#8200,.F.);
#10921=ORIENTED_EDGE('',*,*,#8202,.F.);
#10922=ORIENTED_EDGE('',*,*,#8203,.T.);
#10923=ORIENTED_EDGE('',*,*,#8204,.F.);
#10924=ORIENTED_EDGE('',*,*,#8203,.F.);
#10925=ORIENTED_EDGE('',*,*,#8205,.T.);
#10926=ORIENTED_EDGE('',*,*,#8206,.T.);
#10927=ORIENTED_EDGE('',*,*,#8207,.F.);
#10928=ORIENTED_EDGE('',*,*,#8208,.F.);
#10929=ORIENTED_EDGE('',*,*,#8209,.T.);
#10930=ORIENTED_EDGE('',*,*,#8208,.T.);
#10931=ORIENTED_EDGE('',*,*,#8210,.F.);
#10932=ORIENTED_EDGE('',*,*,#8211,.F.);
#10933=ORIENTED_EDGE('',*,*,#8212,.T.);
#10934=ORIENTED_EDGE('',*,*,#8211,.T.);
#10935=ORIENTED_EDGE('',*,*,#8213,.F.);
#10936=ORIENTED_EDGE('',*,*,#8214,.F.);
#10937=ORIENTED_EDGE('',*,*,#8215,.T.);
#10938=ORIENTED_EDGE('',*,*,#8214,.T.);
#10939=ORIENTED_EDGE('',*,*,#8216,.F.);
#10940=ORIENTED_EDGE('',*,*,#8206,.F.);
#10941=ORIENTED_EDGE('',*,*,#8216,.T.);
#10942=ORIENTED_EDGE('',*,*,#8213,.T.);
#10943=ORIENTED_EDGE('',*,*,#8210,.T.);
#10944=ORIENTED_EDGE('',*,*,#8207,.T.);
#10945=ORIENTED_EDGE('',*,*,#8198,.T.);
#10946=ORIENTED_EDGE('',*,*,#8201,.T.);
#10947=ORIENTED_EDGE('',*,*,#8204,.T.);
#10948=ORIENTED_EDGE('',*,*,#8215,.F.);
#10949=ORIENTED_EDGE('',*,*,#8205,.F.);
#10950=ORIENTED_EDGE('',*,*,#8209,.F.);
#10951=ORIENTED_EDGE('',*,*,#8212,.F.);
#10952=ORIENTED_EDGE('',*,*,#8196,.T.);
#10953=ORIENTED_EDGE('',*,*,#8199,.T.);
#10954=ORIENTED_EDGE('',*,*,#8202,.T.);
#10955=ORIENTED_EDGE('',*,*,#8217,.F.);
#10956=ORIENTED_EDGE('',*,*,#8218,.T.);
#10957=ORIENTED_EDGE('',*,*,#8219,.F.);
#10958=ORIENTED_EDGE('',*,*,#8218,.F.);
#10959=ORIENTED_EDGE('',*,*,#8220,.T.);
#10960=ORIENTED_EDGE('',*,*,#8221,.T.);
#10961=ORIENTED_EDGE('',*,*,#8222,.F.);
#10962=ORIENTED_EDGE('',*,*,#8223,.F.);
#10963=ORIENTED_EDGE('',*,*,#8219,.T.);
#10964=ORIENTED_EDGE('',*,*,#8224,.T.);
#10965=ORIENTED_EDGE('',*,*,#8223,.T.);
#10966=ORIENTED_EDGE('',*,*,#8225,.F.);
#10967=ORIENTED_EDGE('',*,*,#8226,.F.);
#10968=ORIENTED_EDGE('',*,*,#8227,.T.);
#10969=ORIENTED_EDGE('',*,*,#8226,.T.);
#10970=ORIENTED_EDGE('',*,*,#8228,.F.);
#10971=ORIENTED_EDGE('',*,*,#8229,.F.);
#10972=ORIENTED_EDGE('',*,*,#8217,.T.);
#10973=ORIENTED_EDGE('',*,*,#8230,.T.);
#10974=ORIENTED_EDGE('',*,*,#8229,.T.);
#10975=ORIENTED_EDGE('',*,*,#8231,.F.);
#10976=ORIENTED_EDGE('',*,*,#8221,.F.);
#10977=ORIENTED_EDGE('',*,*,#8231,.T.);
#10978=ORIENTED_EDGE('',*,*,#8228,.T.);
#10979=ORIENTED_EDGE('',*,*,#8225,.T.);
#10980=ORIENTED_EDGE('',*,*,#8222,.T.);
#10981=ORIENTED_EDGE('',*,*,#8230,.F.);
#10982=ORIENTED_EDGE('',*,*,#8220,.F.);
#10983=ORIENTED_EDGE('',*,*,#8224,.F.);
#10984=ORIENTED_EDGE('',*,*,#8227,.F.);
#10985=ORIENTED_EDGE('',*,*,#8232,.F.);
#10986=ORIENTED_EDGE('',*,*,#8233,.T.);
#10987=ORIENTED_EDGE('',*,*,#8234,.F.);
#10988=ORIENTED_EDGE('',*,*,#8233,.F.);
#10989=ORIENTED_EDGE('',*,*,#8232,.T.);
#10990=ORIENTED_EDGE('',*,*,#8235,.T.);
#10991=ORIENTED_EDGE('',*,*,#8236,.F.);
#10992=ORIENTED_EDGE('',*,*,#8235,.F.);
#10993=ORIENTED_EDGE('',*,*,#8237,.T.);
#10994=ORIENTED_EDGE('',*,*,#8238,.T.);
#10995=ORIENTED_EDGE('',*,*,#8237,.F.);
#10996=ORIENTED_EDGE('',*,*,#8238,.F.);
#10997=ORIENTED_EDGE('',*,*,#8239,.F.);
#10998=ORIENTED_EDGE('',*,*,#8240,.T.);
#10999=ORIENTED_EDGE('',*,*,#8236,.T.);
#11000=ORIENTED_EDGE('',*,*,#8240,.F.);
#11001=ORIENTED_EDGE('',*,*,#8239,.T.);
#11002=ORIENTED_EDGE('',*,*,#8234,.T.);
#11003=ORIENTED_EDGE('',*,*,#8241,.F.);
#11004=ORIENTED_EDGE('',*,*,#8242,.T.);
#11005=ORIENTED_EDGE('',*,*,#8243,.T.);
#11006=ORIENTED_EDGE('',*,*,#8242,.F.);
#11007=ORIENTED_EDGE('',*,*,#8244,.F.);
#11008=ORIENTED_EDGE('',*,*,#8245,.T.);
#11009=ORIENTED_EDGE('',*,*,#8246,.T.);
#11010=ORIENTED_EDGE('',*,*,#8245,.F.);
#11011=ORIENTED_EDGE('',*,*,#8244,.T.);
#11012=ORIENTED_EDGE('',*,*,#8241,.T.);
#11013=ORIENTED_EDGE('',*,*,#8246,.F.);
#11014=ORIENTED_EDGE('',*,*,#8243,.F.);
#11015=ORIENTED_EDGE('',*,*,#8247,.F.);
#11016=ORIENTED_EDGE('',*,*,#8248,.T.);
#11017=ORIENTED_EDGE('',*,*,#8249,.T.);
#11018=ORIENTED_EDGE('',*,*,#8248,.F.);
#11019=ORIENTED_EDGE('',*,*,#8250,.F.);
#11020=ORIENTED_EDGE('',*,*,#8251,.T.);
#11021=ORIENTED_EDGE('',*,*,#8252,.T.);
#11022=ORIENTED_EDGE('',*,*,#8251,.F.);
#11023=ORIENTED_EDGE('',*,*,#8250,.T.);
#11024=ORIENTED_EDGE('',*,*,#8247,.T.);
#11025=ORIENTED_EDGE('',*,*,#8252,.F.);
#11026=ORIENTED_EDGE('',*,*,#8249,.F.);
#11027=ORIENTED_EDGE('',*,*,#8253,.F.);
#11028=ORIENTED_EDGE('',*,*,#8254,.F.);
#11029=ORIENTED_EDGE('',*,*,#8255,.F.);
#11030=ORIENTED_EDGE('',*,*,#8256,.F.);
#11031=ORIENTED_EDGE('',*,*,#8257,.F.);
#11032=ORIENTED_EDGE('',*,*,#8256,.T.);
#11033=ORIENTED_EDGE('',*,*,#8258,.F.);
#11034=ORIENTED_EDGE('',*,*,#8259,.T.);
#11035=ORIENTED_EDGE('',*,*,#8260,.F.);
#11036=ORIENTED_EDGE('',*,*,#8259,.F.);
#11037=ORIENTED_EDGE('',*,*,#8261,.F.);
#11038=ORIENTED_EDGE('',*,*,#8262,.F.);
#11039=ORIENTED_EDGE('',*,*,#8263,.F.);
#11040=ORIENTED_EDGE('',*,*,#8262,.T.);
#11041=ORIENTED_EDGE('',*,*,#8264,.T.);
#11042=ORIENTED_EDGE('',*,*,#8254,.T.);
#11043=ORIENTED_EDGE('',*,*,#8264,.F.);
#11044=ORIENTED_EDGE('',*,*,#8261,.T.);
#11045=ORIENTED_EDGE('',*,*,#8258,.T.);
#11046=ORIENTED_EDGE('',*,*,#8255,.T.);
#11047=ORIENTED_EDGE('',*,*,#8265,.F.);
#11048=ORIENTED_EDGE('',*,*,#8266,.T.);
#11049=ORIENTED_EDGE('',*,*,#8267,.F.);
#11050=ORIENTED_EDGE('',*,*,#8268,.T.);
#11051=ORIENTED_EDGE('',*,*,#8265,.T.);
#11052=ORIENTED_EDGE('',*,*,#8268,.F.);
#11053=ORIENTED_EDGE('',*,*,#8267,.T.);
#11054=ORIENTED_EDGE('',*,*,#8269,.F.);
#11055=ORIENTED_EDGE('',*,*,#8270,.F.);
#11056=ORIENTED_EDGE('',*,*,#8271,.T.);
#11057=ORIENTED_EDGE('',*,*,#8269,.T.);
#11058=ORIENTED_EDGE('',*,*,#8271,.F.);
#11059=ORIENTED_EDGE('',*,*,#8272,.F.);
#11060=ORIENTED_EDGE('',*,*,#8270,.T.);
#11061=ORIENTED_EDGE('',*,*,#8273,.F.);
#11062=ORIENTED_EDGE('',*,*,#8274,.T.);
#11063=ORIENTED_EDGE('',*,*,#8272,.T.);
#11064=ORIENTED_EDGE('',*,*,#8274,.F.);
#11065=ORIENTED_EDGE('',*,*,#8273,.T.);
#11066=ORIENTED_EDGE('',*,*,#8275,.F.);
#11067=ORIENTED_EDGE('',*,*,#8276,.F.);
#11068=ORIENTED_EDGE('',*,*,#8277,.T.);
#11069=ORIENTED_EDGE('',*,*,#8275,.T.);
#11070=ORIENTED_EDGE('',*,*,#8277,.F.);
#11071=ORIENTED_EDGE('',*,*,#8278,.F.);
#11072=ORIENTED_EDGE('',*,*,#8276,.T.);
#11073=ORIENTED_EDGE('',*,*,#8279,.F.);
#11074=ORIENTED_EDGE('',*,*,#8280,.T.);
#11075=ORIENTED_EDGE('',*,*,#8278,.T.);
#11076=ORIENTED_EDGE('',*,*,#8280,.F.);
#11077=ORIENTED_EDGE('',*,*,#8279,.T.);
#11078=ORIENTED_EDGE('',*,*,#8281,.F.);
#11079=ORIENTED_EDGE('',*,*,#8281,.T.);
#11080=ORIENTED_EDGE('',*,*,#8282,.T.);
#11081=ORIENTED_EDGE('',*,*,#8266,.F.);
#11082=ORIENTED_EDGE('',*,*,#8282,.F.);
#11083=ORIENTED_EDGE('',*,*,#8260,.T.);
#11084=ORIENTED_EDGE('',*,*,#8263,.T.);
#11085=ORIENTED_EDGE('',*,*,#8253,.T.);
#11086=ORIENTED_EDGE('',*,*,#8257,.T.);
#11087=ORIENTED_EDGE('',*,*,#8283,.F.);
#11088=ORIENTED_EDGE('',*,*,#8284,.F.);
#11089=ORIENTED_EDGE('',*,*,#8285,.F.);
#11090=ORIENTED_EDGE('',*,*,#8286,.F.);
#11091=ORIENTED_EDGE('',*,*,#8287,.F.);
#11092=ORIENTED_EDGE('',*,*,#8286,.T.);
#11093=ORIENTED_EDGE('',*,*,#8288,.F.);
#11094=ORIENTED_EDGE('',*,*,#8289,.T.);
#11095=ORIENTED_EDGE('',*,*,#8290,.F.);
#11096=ORIENTED_EDGE('',*,*,#8289,.F.);
#11097=ORIENTED_EDGE('',*,*,#8291,.F.);
#11098=ORIENTED_EDGE('',*,*,#8292,.F.);
#11099=ORIENTED_EDGE('',*,*,#8293,.F.);
#11100=ORIENTED_EDGE('',*,*,#8292,.T.);
#11101=ORIENTED_EDGE('',*,*,#8294,.F.);
#11102=ORIENTED_EDGE('',*,*,#8284,.T.);
#11103=ORIENTED_EDGE('',*,*,#8295,.F.);
#11104=ORIENTED_EDGE('',*,*,#8296,.T.);
#11105=ORIENTED_EDGE('',*,*,#8297,.F.);
#11106=ORIENTED_EDGE('',*,*,#8298,.T.);
#11107=ORIENTED_EDGE('',*,*,#8295,.T.);
#11108=ORIENTED_EDGE('',*,*,#8298,.F.);
#11109=ORIENTED_EDGE('',*,*,#8290,.T.);
#11110=ORIENTED_EDGE('',*,*,#8293,.T.);
#11111=ORIENTED_EDGE('',*,*,#8283,.T.);
#11112=ORIENTED_EDGE('',*,*,#8287,.T.);
#11113=ORIENTED_EDGE('',*,*,#8297,.T.);
#11114=ORIENTED_EDGE('',*,*,#8299,.F.);
#11115=ORIENTED_EDGE('',*,*,#8299,.T.);
#11116=ORIENTED_EDGE('',*,*,#8300,.T.);
#11117=ORIENTED_EDGE('',*,*,#8296,.F.);
#11118=ORIENTED_EDGE('',*,*,#8300,.F.);
#11119=ORIENTED_EDGE('',*,*,#8291,.T.);
#11120=ORIENTED_EDGE('',*,*,#8288,.T.);
#11121=ORIENTED_EDGE('',*,*,#8285,.T.);
#11122=ORIENTED_EDGE('',*,*,#8294,.T.);
#11123=ORIENTED_EDGE('',*,*,#8301,.T.);
#11124=ORIENTED_EDGE('',*,*,#8302,.T.);
#11125=ORIENTED_EDGE('',*,*,#8303,.T.);
#11126=ORIENTED_EDGE('',*,*,#8304,.F.);
#11127=ORIENTED_EDGE('',*,*,#8305,.T.);
#11128=ORIENTED_EDGE('',*,*,#8306,.T.);
#11129=ORIENTED_EDGE('',*,*,#8307,.T.);
#11130=ORIENTED_EDGE('',*,*,#8302,.F.);
#11131=ORIENTED_EDGE('',*,*,#8308,.T.);
#11132=ORIENTED_EDGE('',*,*,#8309,.T.);
#11133=ORIENTED_EDGE('',*,*,#8310,.T.);
#11134=ORIENTED_EDGE('',*,*,#8306,.F.);
#11135=ORIENTED_EDGE('',*,*,#8311,.T.);
#11136=ORIENTED_EDGE('',*,*,#8312,.T.);
#11137=ORIENTED_EDGE('',*,*,#8313,.T.);
#11138=ORIENTED_EDGE('',*,*,#8309,.F.);
#11139=ORIENTED_EDGE('',*,*,#8314,.T.);
#11140=ORIENTED_EDGE('',*,*,#8315,.T.);
#11141=ORIENTED_EDGE('',*,*,#8316,.T.);
#11142=ORIENTED_EDGE('',*,*,#8312,.F.);
#11143=ORIENTED_EDGE('',*,*,#8317,.T.);
#11144=ORIENTED_EDGE('',*,*,#8304,.T.);
#11145=ORIENTED_EDGE('',*,*,#8318,.T.);
#11146=ORIENTED_EDGE('',*,*,#8315,.F.);
#11147=ORIENTED_EDGE('',*,*,#8317,.F.);
#11148=ORIENTED_EDGE('',*,*,#8314,.F.);
#11149=ORIENTED_EDGE('',*,*,#8311,.F.);
#11150=ORIENTED_EDGE('',*,*,#8308,.F.);
#11151=ORIENTED_EDGE('',*,*,#8305,.F.);
#11152=ORIENTED_EDGE('',*,*,#8301,.F.);
#11153=ORIENTED_EDGE('',*,*,#8318,.F.);
#11154=ORIENTED_EDGE('',*,*,#8303,.F.);
#11155=ORIENTED_EDGE('',*,*,#8307,.F.);
#11156=ORIENTED_EDGE('',*,*,#8310,.F.);
#11157=ORIENTED_EDGE('',*,*,#8313,.F.);
#11158=ORIENTED_EDGE('',*,*,#8316,.F.);
#11159=ORIENTED_EDGE('',*,*,#8319,.F.);
#11160=ORIENTED_EDGE('',*,*,#8320,.F.);
#11161=ORIENTED_EDGE('',*,*,#8321,.F.);
#11162=ORIENTED_EDGE('',*,*,#8322,.T.);
#11163=ORIENTED_EDGE('',*,*,#8320,.T.);
#11164=ORIENTED_EDGE('',*,*,#8322,.F.);
#11165=ORIENTED_EDGE('',*,*,#8323,.F.);
#11166=ORIENTED_EDGE('',*,*,#8324,.T.);
#11167=ORIENTED_EDGE('',*,*,#8321,.T.);
#11168=ORIENTED_EDGE('',*,*,#8324,.F.);
#11169=ORIENTED_EDGE('',*,*,#8325,.F.);
#11170=ORIENTED_EDGE('',*,*,#8326,.T.);
#11171=ORIENTED_EDGE('',*,*,#8323,.T.);
#11172=ORIENTED_EDGE('',*,*,#8326,.F.);
#11173=ORIENTED_EDGE('',*,*,#8325,.T.);
#11174=ORIENTED_EDGE('',*,*,#8327,.F.);
#11175=ORIENTED_EDGE('',*,*,#8328,.F.);
#11176=ORIENTED_EDGE('',*,*,#8329,.T.);
#11177=ORIENTED_EDGE('',*,*,#8327,.T.);
#11178=ORIENTED_EDGE('',*,*,#8329,.F.);
#11179=ORIENTED_EDGE('',*,*,#8319,.T.);
#11180=ORIENTED_EDGE('',*,*,#8330,.T.);
#11181=ORIENTED_EDGE('',*,*,#8328,.T.);
#11182=ORIENTED_EDGE('',*,*,#8330,.F.);
#11183=ORIENTED_EDGE('',*,*,#8331,.F.);
#11184=ORIENTED_EDGE('',*,*,#8332,.T.);
#11185=ORIENTED_EDGE('',*,*,#8333,.F.);
#11186=ORIENTED_EDGE('',*,*,#8332,.F.);
#11187=ORIENTED_EDGE('',*,*,#8334,.F.);
#11188=ORIENTED_EDGE('',*,*,#8335,.F.);
#11189=ORIENTED_EDGE('',*,*,#8336,.F.);
#11190=ORIENTED_EDGE('',*,*,#8337,.T.);
#11191=ORIENTED_EDGE('',*,*,#8337,.F.);
#11192=ORIENTED_EDGE('',*,*,#8338,.F.);
#11193=ORIENTED_EDGE('',*,*,#8339,.F.);
#11194=ORIENTED_EDGE('',*,*,#8340,.F.);
#11195=ORIENTED_EDGE('',*,*,#8331,.T.);
#11196=ORIENTED_EDGE('',*,*,#8341,.T.);
#11197=ORIENTED_EDGE('',*,*,#8336,.T.);
#11198=ORIENTED_EDGE('',*,*,#8342,.F.);
#11199=ORIENTED_EDGE('',*,*,#8343,.T.);
#11200=ORIENTED_EDGE('',*,*,#8338,.T.);
#11201=ORIENTED_EDGE('',*,*,#8341,.F.);
#11202=ORIENTED_EDGE('',*,*,#8344,.T.);
#11203=ORIENTED_EDGE('',*,*,#8345,.F.);
#11204=ORIENTED_EDGE('',*,*,#8344,.F.);
#11205=ORIENTED_EDGE('',*,*,#8346,.F.);
#11206=ORIENTED_EDGE('',*,*,#8339,.T.);
#11207=ORIENTED_EDGE('',*,*,#8343,.F.);
#11208=ORIENTED_EDGE('',*,*,#8347,.F.);
#11209=ORIENTED_EDGE('',*,*,#8334,.T.);
#11210=ORIENTED_EDGE('',*,*,#8340,.T.);
#11211=ORIENTED_EDGE('',*,*,#8346,.T.);
#11212=ORIENTED_EDGE('',*,*,#8348,.F.);
#11213=ORIENTED_EDGE('',*,*,#8348,.T.);
#11214=ORIENTED_EDGE('',*,*,#8347,.T.);
#11215=ORIENTED_EDGE('',*,*,#8342,.T.);
#11216=ORIENTED_EDGE('',*,*,#8335,.T.);
#11217=ORIENTED_EDGE('',*,*,#8333,.T.);
#11218=ORIENTED_EDGE('',*,*,#8345,.T.);
#11219=ORIENTED_EDGE('',*,*,#8349,.F.);
#11220=ORIENTED_EDGE('',*,*,#8350,.T.);
#11221=ORIENTED_EDGE('',*,*,#8351,.T.);
#11222=ORIENTED_EDGE('',*,*,#8350,.F.);
#11223=ORIENTED_EDGE('',*,*,#8349,.T.);
#11224=ORIENTED_EDGE('',*,*,#8351,.F.);
#11225=ORIENTED_EDGE('',*,*,#8352,.F.);
#11226=ORIENTED_EDGE('',*,*,#8353,.T.);
#11227=ORIENTED_EDGE('',*,*,#8354,.T.);
#11228=ORIENTED_EDGE('',*,*,#8353,.F.);
#11229=ORIENTED_EDGE('',*,*,#8355,.F.);
#11230=ORIENTED_EDGE('',*,*,#8356,.T.);
#11231=ORIENTED_EDGE('',*,*,#8357,.T.);
#11232=ORIENTED_EDGE('',*,*,#8356,.F.);
#11233=ORIENTED_EDGE('',*,*,#8355,.T.);
#11234=ORIENTED_EDGE('',*,*,#8352,.T.);
#11235=ORIENTED_EDGE('',*,*,#8357,.F.);
#11236=ORIENTED_EDGE('',*,*,#8354,.F.);
#11237=ORIENTED_EDGE('',*,*,#8358,.F.);
#11238=ORIENTED_EDGE('',*,*,#8359,.T.);
#11239=ORIENTED_EDGE('',*,*,#8360,.T.);
#11240=ORIENTED_EDGE('',*,*,#8359,.F.);
#11241=ORIENTED_EDGE('',*,*,#8361,.F.);
#11242=ORIENTED_EDGE('',*,*,#8362,.T.);
#11243=ORIENTED_EDGE('',*,*,#8363,.T.);
#11244=ORIENTED_EDGE('',*,*,#8362,.F.);
#11245=ORIENTED_EDGE('',*,*,#8361,.T.);
#11246=ORIENTED_EDGE('',*,*,#8358,.T.);
#11247=ORIENTED_EDGE('',*,*,#8363,.F.);
#11248=ORIENTED_EDGE('',*,*,#8360,.F.);
#11249=ORIENTED_EDGE('',*,*,#8364,.F.);
#11250=ORIENTED_EDGE('',*,*,#8365,.T.);
#11251=ORIENTED_EDGE('',*,*,#8366,.T.);
#11252=ORIENTED_EDGE('',*,*,#8365,.F.);
#11253=ORIENTED_EDGE('',*,*,#8367,.F.);
#11254=ORIENTED_EDGE('',*,*,#8368,.T.);
#11255=ORIENTED_EDGE('',*,*,#8369,.T.);
#11256=ORIENTED_EDGE('',*,*,#8368,.F.);
#11257=ORIENTED_EDGE('',*,*,#8367,.T.);
#11258=ORIENTED_EDGE('',*,*,#8364,.T.);
#11259=ORIENTED_EDGE('',*,*,#8369,.F.);
#11260=ORIENTED_EDGE('',*,*,#8366,.F.);
#11261=ORIENTED_EDGE('',*,*,#8370,.F.);
#11262=ORIENTED_EDGE('',*,*,#8371,.T.);
#11263=ORIENTED_EDGE('',*,*,#8372,.T.);
#11264=ORIENTED_EDGE('',*,*,#8371,.F.);
#11265=ORIENTED_EDGE('',*,*,#8370,.T.);
#11266=ORIENTED_EDGE('',*,*,#8372,.F.);
#11267=CYLINDRICAL_SURFACE('',#13679,0.165);
#11268=CYLINDRICAL_SURFACE('',#13682,0.165);
#11269=CYLINDRICAL_SURFACE('',#13685,0.164999999999999);
#11270=CYLINDRICAL_SURFACE('',#13688,0.164999999999999);
#11271=CYLINDRICAL_SURFACE('',#13691,0.210000000000001);
#11272=CYLINDRICAL_SURFACE('',#13694,0.210000000000001);
#11273=CYLINDRICAL_SURFACE('',#13697,0.210000000000001);
#11274=CYLINDRICAL_SURFACE('',#13700,0.210000000000001);
#11275=CYLINDRICAL_SURFACE('',#13703,0.21);
#11276=CYLINDRICAL_SURFACE('',#13706,0.21);
#11277=CYLINDRICAL_SURFACE('',#13709,0.21);
#11278=CYLINDRICAL_SURFACE('',#13712,0.21);
#11279=CYLINDRICAL_SURFACE('',#13736,0.165);
#11280=CYLINDRICAL_SURFACE('',#13739,0.165);
#11281=CYLINDRICAL_SURFACE('',#13742,0.165);
#11282=CYLINDRICAL_SURFACE('',#13745,0.605);
#11283=CYLINDRICAL_SURFACE('',#13748,0.275);
#11284=CYLINDRICAL_SURFACE('',#13751,0.275);
#11285=CYLINDRICAL_SURFACE('',#13754,0.275);
#11286=CYLINDRICAL_SURFACE('',#13757,0.275);
#11287=CYLINDRICAL_SURFACE('',#13771,0.164999999999999);
#11288=CYLINDRICAL_SURFACE('',#13774,0.164999999999999);
#11289=CYLINDRICAL_SURFACE('',#13777,0.164999999999999);
#11290=CYLINDRICAL_SURFACE('',#13780,0.605);
#11291=CYLINDRICAL_SURFACE('',#13783,0.274999999999999);
#11292=CYLINDRICAL_SURFACE('',#13786,0.274999999999999);
#11293=CYLINDRICAL_SURFACE('',#13789,0.275);
#11294=CYLINDRICAL_SURFACE('',#13792,0.275);
#11295=CYLINDRICAL_SURFACE('',#13806,0.165);
#11296=CYLINDRICAL_SURFACE('',#13810,0.225);
#11297=CYLINDRICAL_SURFACE('',#13813,0.225);
#11298=CYLINDRICAL_SURFACE('',#13816,0.225);
#11299=CYLINDRICAL_SURFACE('',#13825,1.5);
#11300=CYLINDRICAL_SURFACE('',#13826,0.6);
#11301=CYLINDRICAL_SURFACE('',#13828,0.6);
#11302=CYLINDRICAL_SURFACE('',#13833,0.605);
#11303=CYLINDRICAL_SURFACE('',#13836,0.8);
#11304=CYLINDRICAL_SURFACE('',#13842,0.605);
#11305=CYLINDRICAL_SURFACE('',#13845,0.8);
#11306=CYLINDRICAL_SURFACE('',#13851,0.225);
#11307=CYLINDRICAL_SURFACE('',#13854,1.);
#11308=CYLINDRICAL_SURFACE('',#13860,0.164999999999999);
#11309=CYLINDRICAL_SURFACE('',#13864,0.225000000000001);
#11310=CYLINDRICAL_SURFACE('',#13867,0.225000000000001);
#11311=CYLINDRICAL_SURFACE('',#13870,0.225000000000001);
#11312=CYLINDRICAL_SURFACE('',#13879,1.5);
#11313=CYLINDRICAL_SURFACE('',#13880,0.600000000000001);
#11314=CYLINDRICAL_SURFACE('',#13882,0.600000000000001);
#11315=CYLINDRICAL_SURFACE('',#13887,0.605);
#11316=CYLINDRICAL_SURFACE('',#13890,0.800000000000001);
#11317=CYLINDRICAL_SURFACE('',#13896,0.605);
#11318=CYLINDRICAL_SURFACE('',#13899,0.800000000000001);
#11319=CYLINDRICAL_SURFACE('',#13905,0.225000000000001);
#11320=CYLINDRICAL_SURFACE('',#13908,1.);
#11321=CYLINDRICAL_SURFACE('',#13914,0.164999999999999);
#11322=CYLINDRICAL_SURFACE('',#13917,0.165);
#11323=CYLINDRICAL_SURFACE('',#13926,0.4);
#11324=CYLINDRICAL_SURFACE('',#13931,0.225);
#11325=CYLINDRICAL_SURFACE('',#13933,0.4);
#11326=CYLINDRICAL_SURFACE('',#13937,0.225);
#11327=CYLINDRICAL_SURFACE('',#13939,1.6);
#11328=CYLINDRICAL_SURFACE('',#13941,0.605);
#11329=CYLINDRICAL_SURFACE('',#13943,0.605);
#11330=CYLINDRICAL_SURFACE('',#13951,0.225);
#11331=CYLINDRICAL_SURFACE('',#13954,0.225);
#11332=CYLINDRICAL_SURFACE('',#13957,0.61);
#11333=CYLINDRICAL_SURFACE('',#13960,0.61);
#11334=CYLINDRICAL_SURFACE('',#13967,2.1);
#11335=CYLINDRICAL_SURFACE('',#13969,2.1);
#11336=CYLINDRICAL_SURFACE('',#13971,1.02);
#11337=CYLINDRICAL_SURFACE('',#13978,0.35);
#11338=CYLINDRICAL_SURFACE('',#13981,0.199999999999999);
#11339=CYLINDRICAL_SURFACE('',#13988,0.35);
#11340=CYLINDRICAL_SURFACE('',#13991,0.2);
#11341=CYLINDRICAL_SURFACE('',#13995,0.225);
#11342=CYLINDRICAL_SURFACE('',#13998,0.225);
#11343=CYLINDRICAL_SURFACE('',#14001,0.61);
#11344=CYLINDRICAL_SURFACE('',#14004,0.61);
#11345=CYLINDRICAL_SURFACE('',#14011,2.1);
#11346=CYLINDRICAL_SURFACE('',#14013,2.1);
#11347=CYLINDRICAL_SURFACE('',#14015,1.02);
#11348=CYLINDRICAL_SURFACE('',#14022,0.35);
#11349=CYLINDRICAL_SURFACE('',#14025,0.199999999999999);
#11350=CYLINDRICAL_SURFACE('',#14032,0.35);
#11351=CYLINDRICAL_SURFACE('',#14035,0.2);
#11352=CYLINDRICAL_SURFACE('',#14039,0.164999999999999);
#11353=CYLINDRICAL_SURFACE('',#14042,0.165);
#11354=CYLINDRICAL_SURFACE('',#14051,0.4);
#11355=CYLINDRICAL_SURFACE('',#14056,0.225);
#11356=CYLINDRICAL_SURFACE('',#14058,0.4);
#11357=CYLINDRICAL_SURFACE('',#14062,0.225);
#11358=CYLINDRICAL_SURFACE('',#14064,1.6);
#11359=CYLINDRICAL_SURFACE('',#14066,0.605);
#11360=CYLINDRICAL_SURFACE('',#14068,0.605);
#11361=CYLINDRICAL_SURFACE('',#14076,0.225);
#11362=CYLINDRICAL_SURFACE('',#14079,0.225);
#11363=CYLINDRICAL_SURFACE('',#14082,0.61);
#11364=CYLINDRICAL_SURFACE('',#14085,0.61);
#11365=CYLINDRICAL_SURFACE('',#14092,2.1);
#11366=CYLINDRICAL_SURFACE('',#14094,2.1);
#11367=CYLINDRICAL_SURFACE('',#14096,1.02);
#11368=CYLINDRICAL_SURFACE('',#14103,0.35);
#11369=CYLINDRICAL_SURFACE('',#14106,0.199999999999999);
#11370=CYLINDRICAL_SURFACE('',#14113,0.35);
#11371=CYLINDRICAL_SURFACE('',#14116,0.2);
#11372=CYLINDRICAL_SURFACE('',#14120,0.225);
#11373=CYLINDRICAL_SURFACE('',#14123,0.225);
#11374=CYLINDRICAL_SURFACE('',#14126,0.61);
#11375=CYLINDRICAL_SURFACE('',#14129,0.61);
#11376=CYLINDRICAL_SURFACE('',#14136,2.1);
#11377=CYLINDRICAL_SURFACE('',#14138,2.1);
#11378=CYLINDRICAL_SURFACE('',#14140,1.02);
#11379=CYLINDRICAL_SURFACE('',#14147,0.35);
#11380=CYLINDRICAL_SURFACE('',#14150,0.199999999999999);
#11381=CYLINDRICAL_SURFACE('',#14157,0.35);
#11382=CYLINDRICAL_SURFACE('',#14160,0.2);
#11383=CYLINDRICAL_SURFACE('',#14164,0.6);
#11384=CYLINDRICAL_SURFACE('',#14170,0.6);
#11385=CYLINDRICAL_SURFACE('',#14180,0.425);
#11386=CYLINDRICAL_SURFACE('',#14188,0.24505);
#11387=CYLINDRICAL_SURFACE('',#14203,0.164999999999999);
#11388=CYLINDRICAL_SURFACE('',#14206,0.164999999999999);
#11389=CYLINDRICAL_SURFACE('',#14209,0.164999999999999);
#11390=CYLINDRICAL_SURFACE('',#14212,0.164999999999999);
#11391=CYLINDRICAL_SURFACE('',#14215,1.6);
#11392=CYLINDRICAL_SURFACE('',#14218,2.2);
#11393=CYLINDRICAL_SURFACE('',#14229,0.165);
#11394=CYLINDRICAL_SURFACE('',#14231,0.165);
#11395=CYLINDRICAL_SURFACE('',#14233,0.165);
#11396=CYLINDRICAL_SURFACE('',#14235,0.165);
#11397=CYLINDRICAL_SURFACE('',#14237,1.6);
#11398=CYLINDRICAL_SURFACE('',#14239,2.2);
#11399=CYLINDRICAL_SURFACE('',#14244,0.225);
#11400=CYLINDRICAL_SURFACE('',#14247,0.225);
#11401=CYLINDRICAL_SURFACE('',#14250,0.225);
#11402=CYLINDRICAL_SURFACE('',#14253,0.225);
#11403=CYLINDRICAL_SURFACE('',#14256,1.02);
#11404=CYLINDRICAL_SURFACE('',#14259,2.2);
#11405=CYLINDRICAL_SURFACE('',#14268,0.35);
#11406=CYLINDRICAL_SURFACE('',#14271,0.2);
#11407=CYLINDRICAL_SURFACE('',#14278,0.35);
#11408=CYLINDRICAL_SURFACE('',#14281,0.2);
#11409=CYLINDRICAL_SURFACE('',#14288,0.35);
#11410=CYLINDRICAL_SURFACE('',#14291,0.2);
#11411=CYLINDRICAL_SURFACE('',#14298,0.35);
#11412=CYLINDRICAL_SURFACE('',#14301,0.2);
#11413=CYLINDRICAL_SURFACE('',#14305,0.225);
#11414=CYLINDRICAL_SURFACE('',#14308,0.225);
#11415=CYLINDRICAL_SURFACE('',#14311,0.225);
#11416=CYLINDRICAL_SURFACE('',#14314,0.225);
#11417=CYLINDRICAL_SURFACE('',#14317,1.02);
#11418=CYLINDRICAL_SURFACE('',#14320,2.2);
#11419=CYLINDRICAL_SURFACE('',#14329,0.35);
#11420=CYLINDRICAL_SURFACE('',#14332,0.2);
#11421=CYLINDRICAL_SURFACE('',#14339,0.35);
#11422=CYLINDRICAL_SURFACE('',#14342,0.2);
#11423=CYLINDRICAL_SURFACE('',#14349,0.35);
#11424=CYLINDRICAL_SURFACE('',#14352,0.2);
#11425=CYLINDRICAL_SURFACE('',#14359,0.35);
#11426=CYLINDRICAL_SURFACE('',#14362,0.2);
#11427=CYLINDRICAL_SURFACE('',#14366,0.225);
#11428=CYLINDRICAL_SURFACE('',#14369,0.225);
#11429=CYLINDRICAL_SURFACE('',#14372,0.225);
#11430=CYLINDRICAL_SURFACE('',#14375,0.225);
#11431=CYLINDRICAL_SURFACE('',#14378,1.02);
#11432=CYLINDRICAL_SURFACE('',#14381,2.2);
#11433=CYLINDRICAL_SURFACE('',#14390,0.35);
#11434=CYLINDRICAL_SURFACE('',#14393,0.199999999999999);
#11435=CYLINDRICAL_SURFACE('',#14400,0.35);
#11436=CYLINDRICAL_SURFACE('',#14403,0.199999999999999);
#11437=CYLINDRICAL_SURFACE('',#14410,0.35);
#11438=CYLINDRICAL_SURFACE('',#14413,0.199999999999999);
#11439=CYLINDRICAL_SURFACE('',#14420,0.35);
#11440=CYLINDRICAL_SURFACE('',#14423,0.199999999999999);
#11441=CYLINDRICAL_SURFACE('',#14427,0.225);
#11442=CYLINDRICAL_SURFACE('',#14430,0.225);
#11443=CYLINDRICAL_SURFACE('',#14433,0.225);
#11444=CYLINDRICAL_SURFACE('',#14436,0.225);
#11445=CYLINDRICAL_SURFACE('',#14439,1.02);
#11446=CYLINDRICAL_SURFACE('',#14442,2.2);
#11447=CYLINDRICAL_SURFACE('',#14451,0.35);
#11448=CYLINDRICAL_SURFACE('',#14454,0.199999999999999);
#11449=CYLINDRICAL_SURFACE('',#14461,0.35);
#11450=CYLINDRICAL_SURFACE('',#14464,0.199999999999999);
#11451=CYLINDRICAL_SURFACE('',#14471,0.35);
#11452=CYLINDRICAL_SURFACE('',#14474,0.199999999999999);
#11453=CYLINDRICAL_SURFACE('',#14481,0.35);
#11454=CYLINDRICAL_SURFACE('',#14484,0.199999999999999);
#11455=CYLINDRICAL_SURFACE('',#14489,0.164999999999999);
#11456=CYLINDRICAL_SURFACE('',#14492,0.164999999999999);
#11457=CYLINDRICAL_SURFACE('',#14495,0.164999999999999);
#11458=CYLINDRICAL_SURFACE('',#14498,0.164999999999999);
#11459=CYLINDRICAL_SURFACE('',#14501,1.6);
#11460=CYLINDRICAL_SURFACE('',#14504,2.2);
#11461=CYLINDRICAL_SURFACE('',#14515,0.164999999999999);
#11462=CYLINDRICAL_SURFACE('',#14517,0.164999999999999);
#11463=CYLINDRICAL_SURFACE('',#14519,0.164999999999999);
#11464=CYLINDRICAL_SURFACE('',#14521,0.164999999999999);
#11465=CYLINDRICAL_SURFACE('',#14523,1.6);
#11466=CYLINDRICAL_SURFACE('',#14525,2.2);
#11467=CYLINDRICAL_SURFACE('',#14530,0.225000000000001);
#11468=CYLINDRICAL_SURFACE('',#14533,0.225000000000001);
#11469=CYLINDRICAL_SURFACE('',#14536,0.225000000000001);
#11470=CYLINDRICAL_SURFACE('',#14539,0.225000000000001);
#11471=CYLINDRICAL_SURFACE('',#14542,1.02);
#11472=CYLINDRICAL_SURFACE('',#14545,2.2);
#11473=CYLINDRICAL_SURFACE('',#14554,0.350000000000001);
#11474=CYLINDRICAL_SURFACE('',#14557,0.199999999999999);
#11475=CYLINDRICAL_SURFACE('',#14564,0.350000000000001);
#11476=CYLINDRICAL_SURFACE('',#14567,0.199999999999999);
#11477=CYLINDRICAL_SURFACE('',#14574,0.350000000000001);
#11478=CYLINDRICAL_SURFACE('',#14577,0.199999999999999);
#11479=CYLINDRICAL_SURFACE('',#14584,0.350000000000001);
#11480=CYLINDRICAL_SURFACE('',#14587,0.199999999999999);
#11481=CYLINDRICAL_SURFACE('',#14591,0.225000000000001);
#11482=CYLINDRICAL_SURFACE('',#14594,0.225000000000001);
#11483=CYLINDRICAL_SURFACE('',#14597,0.225000000000001);
#11484=CYLINDRICAL_SURFACE('',#14600,0.225000000000001);
#11485=CYLINDRICAL_SURFACE('',#14603,1.02);
#11486=CYLINDRICAL_SURFACE('',#14606,2.2);
#11487=CYLINDRICAL_SURFACE('',#14615,0.350000000000001);
#11488=CYLINDRICAL_SURFACE('',#14618,0.199999999999999);
#11489=CYLINDRICAL_SURFACE('',#14625,0.350000000000001);
#11490=CYLINDRICAL_SURFACE('',#14628,0.199999999999999);
#11491=CYLINDRICAL_SURFACE('',#14635,0.350000000000001);
#11492=CYLINDRICAL_SURFACE('',#14638,0.199999999999999);
#11493=CYLINDRICAL_SURFACE('',#14645,0.350000000000001);
#11494=CYLINDRICAL_SURFACE('',#14648,0.199999999999999);
#11495=CYLINDRICAL_SURFACE('',#14652,0.225000000000001);
#11496=CYLINDRICAL_SURFACE('',#14655,0.225000000000001);
#11497=CYLINDRICAL_SURFACE('',#14658,0.225000000000001);
#11498=CYLINDRICAL_SURFACE('',#14661,0.225000000000001);
#11499=CYLINDRICAL_SURFACE('',#14664,1.02);
#11500=CYLINDRICAL_SURFACE('',#14667,2.2);
#11501=CYLINDRICAL_SURFACE('',#14676,0.350000000000001);
#11502=CYLINDRICAL_SURFACE('',#14679,0.199999999999999);
#11503=CYLINDRICAL_SURFACE('',#14686,0.350000000000001);
#11504=CYLINDRICAL_SURFACE('',#14689,0.199999999999999);
#11505=CYLINDRICAL_SURFACE('',#14696,0.350000000000001);
#11506=CYLINDRICAL_SURFACE('',#14699,0.199999999999999);
#11507=CYLINDRICAL_SURFACE('',#14706,0.350000000000001);
#11508=CYLINDRICAL_SURFACE('',#14709,0.199999999999999);
#11509=CYLINDRICAL_SURFACE('',#14713,0.225000000000001);
#11510=CYLINDRICAL_SURFACE('',#14716,0.225000000000001);
#11511=CYLINDRICAL_SURFACE('',#14719,0.225000000000001);
#11512=CYLINDRICAL_SURFACE('',#14722,0.225000000000001);
#11513=CYLINDRICAL_SURFACE('',#14725,1.02);
#11514=CYLINDRICAL_SURFACE('',#14728,2.2);
#11515=CYLINDRICAL_SURFACE('',#14737,0.350000000000001);
#11516=CYLINDRICAL_SURFACE('',#14740,0.199999999999999);
#11517=CYLINDRICAL_SURFACE('',#14747,0.350000000000001);
#11518=CYLINDRICAL_SURFACE('',#14750,0.199999999999999);
#11519=CYLINDRICAL_SURFACE('',#14757,0.350000000000001);
#11520=CYLINDRICAL_SURFACE('',#14760,0.199999999999999);
#11521=CYLINDRICAL_SURFACE('',#14767,0.350000000000001);
#11522=CYLINDRICAL_SURFACE('',#14770,0.199999999999999);
#11523=CYLINDRICAL_SURFACE('',#14781,1.070235);
#11524=CYLINDRICAL_SURFACE('',#14783,0.6);
#11525=CYLINDRICAL_SURFACE('',#14789,1.070235);
#11526=CYLINDRICAL_SURFACE('',#14801,1.129765);
#11527=CYLINDRICAL_SURFACE('',#14808,1.6);
#11528=CYLINDRICAL_SURFACE('',#14813,1.129765);
#11529=CYLINDRICAL_SURFACE('',#14833,1.123812);
#11530=CYLINDRICAL_SURFACE('',#14869,1.076188);
#11531=CYLINDRICAL_SURFACE('',#14883,1.119765);
#11532=CYLINDRICAL_SURFACE('',#14887,1.085235);
#11533=CYLINDRICAL_SURFACE('',#14891,1.119765);
#11534=CYLINDRICAL_SURFACE('',#14895,1.085235);
#11535=CYLINDRICAL_SURFACE('',#14949,0.164999999999999);
#11536=CYLINDRICAL_SURFACE('',#14952,0.164999999999999);
#11537=CYLINDRICAL_SURFACE('',#14955,0.164999999999999);
#11538=CYLINDRICAL_SURFACE('',#14958,0.605);
#11539=CYLINDRICAL_SURFACE('',#14961,0.164999999999999);
#11540=CYLINDRICAL_SURFACE('',#14964,0.164999999999999);
#11541=CYLINDRICAL_SURFACE('',#14967,0.164999999999999);
#11542=CYLINDRICAL_SURFACE('',#14970,0.605);
#11543=CYLINDRICAL_SURFACE('',#14976,1.8);
#11544=CYLINDRICAL_SURFACE('',#14979,1.8);
#11545=CYLINDRICAL_SURFACE('',#14988,1.8);
#11546=CYLINDRICAL_SURFACE('',#15013,0.164999999999999);
#11547=CYLINDRICAL_SURFACE('',#15017,0.225);
#11548=CYLINDRICAL_SURFACE('',#15020,0.225);
#11549=CYLINDRICAL_SURFACE('',#15023,0.225);
#11550=CYLINDRICAL_SURFACE('',#15032,1.5);
#11551=CYLINDRICAL_SURFACE('',#15033,0.6);
#11552=CYLINDRICAL_SURFACE('',#15035,0.6);
#11553=CYLINDRICAL_SURFACE('',#15040,0.605);
#11554=CYLINDRICAL_SURFACE('',#15043,0.800000000000001);
#11555=CYLINDRICAL_SURFACE('',#15049,0.605);
#11556=CYLINDRICAL_SURFACE('',#15052,0.800000000000001);
#11557=CYLINDRICAL_SURFACE('',#15058,0.605);
#11558=CYLINDRICAL_SURFACE('',#15061,0.800000000000001);
#11559=CYLINDRICAL_SURFACE('',#15067,0.225);
#11560=CYLINDRICAL_SURFACE('',#15070,1.);
#11561=CYLINDRICAL_SURFACE('',#15076,0.164999999999999);
#11562=CYLINDRICAL_SURFACE('',#15080,0.225000000000001);
#11563=CYLINDRICAL_SURFACE('',#15083,0.225000000000001);
#11564=CYLINDRICAL_SURFACE('',#15086,0.225000000000001);
#11565=CYLINDRICAL_SURFACE('',#15095,1.5);
#11566=CYLINDRICAL_SURFACE('',#15096,0.600000000000001);
#11567=CYLINDRICAL_SURFACE('',#15098,0.600000000000001);
#11568=CYLINDRICAL_SURFACE('',#15103,0.605);
#11569=CYLINDRICAL_SURFACE('',#15106,0.800000000000001);
#11570=CYLINDRICAL_SURFACE('',#15112,0.605);
#11571=CYLINDRICAL_SURFACE('',#15115,0.800000000000001);
#11572=CYLINDRICAL_SURFACE('',#15121,0.225000000000001);
#11573=CYLINDRICAL_SURFACE('',#15124,1.);
#11574=CYLINDRICAL_SURFACE('',#15134,0.35);
#11575=CYLINDRICAL_SURFACE('',#15142,0.1954);
#11576=CYLINDRICAL_SURFACE('',#15228,0.5);
#11577=CYLINDRICAL_SURFACE('',#15231,1.05);
#11578=CYLINDRICAL_SURFACE('',#15234,1.05);
#11579=CYLINDRICAL_SURFACE('',#15244,0.65);
#11580=CYLINDRICAL_SURFACE('',#15247,0.8);
#11581=CYLINDRICAL_SURFACE('',#15250,0.8);
#11582=CYLINDRICAL_SURFACE('',#15260,0.65);
#11583=CYLINDRICAL_SURFACE('',#15263,0.8);
#11584=CYLINDRICAL_SURFACE('',#15266,0.8);
#11585=CYLINDRICAL_SURFACE('',#15276,0.305);
#11586=CYLINDRICAL_SURFACE('',#15286,0.165);
#11587=CYLINDRICAL_SURFACE('',#15293,0.5);
#11588=CYLINDRICAL_SURFACE('',#15296,0.3);
#11589=CYLINDRICAL_SURFACE('',#15300,0.225);
#11590=CYLINDRICAL_SURFACE('',#15303,0.6);
#11591=CYLINDRICAL_SURFACE('',#15309,0.305);
#11592=CYLINDRICAL_SURFACE('',#15312,0.45);
#11593=CYLINDRICAL_SURFACE('',#15329,1.05);
#11594=CYLINDRICAL_SURFACE('',#15333,1.);
#11595=CYLINDRICAL_SURFACE('',#15337,1.05);
#11596=CYLINDRICAL_SURFACE('',#15341,1.);
#11597=CYLINDRICAL_SURFACE('',#15345,1.05);
#11598=CYLINDRICAL_SURFACE('',#15349,0.9);
#11599=CYLINDRICAL_SURFACE('',#15362,0.895);
#11600=CYLINDRICAL_SURFACE('',#15366,0.605);
#11601=CYLINDRICAL_SURFACE('',#15384,0.35);
#11602=CYLINDRICAL_SURFACE('',#15392,0.1954);
#11603=CYLINDRICAL_SURFACE('',#15405,0.605);
#11604=CYLINDRICAL_SURFACE('',#15408,1.1);
#11605=CYLINDRICAL_SURFACE('',#15415,0.305);
#11606=CYLINDRICAL_SURFACE('',#15417,0.8);
#11607=CYLINDRICAL_SURFACE('',#15424,0.6);
#11608=CYLINDRICAL_SURFACE('',#15430,0.6);
#11609=CYLINDRICAL_SURFACE('',#15433,0.9);
#11610=CYLINDRICAL_SURFACE('',#15439,0.6);
#11611=CYLINDRICAL_SURFACE('',#15442,0.9);
#11612=CYLINDRICAL_SURFACE('',#15448,0.6);
#11613=CYLINDRICAL_SURFACE('',#15451,2.);
#11614=CYLINDRICAL_SURFACE('',#15457,0.4);
#11615=ADVANCED_FACE('',(#1890),#11267,.F.);
#11616=ADVANCED_FACE('',(#1891),#11268,.F.);
#11617=ADVANCED_FACE('',(#1892),#11269,.F.);
#11618=ADVANCED_FACE('',(#1893),#11270,.F.);
#11619=ADVANCED_FACE('',(#1894),#11271,.F.);
#11620=ADVANCED_FACE('',(#1895),#11272,.F.);
#11621=ADVANCED_FACE('',(#1896),#11273,.F.);
#11622=ADVANCED_FACE('',(#1897),#11274,.F.);
#11623=ADVANCED_FACE('',(#1898),#11275,.F.);
#11624=ADVANCED_FACE('',(#1899),#11276,.F.);
#11625=ADVANCED_FACE('',(#1900),#11277,.F.);
#11626=ADVANCED_FACE('',(#1901),#11278,.F.);
#11627=ADVANCED_FACE('',(#1902),#1492,.T.);
#11628=ADVANCED_FACE('',(#1903),#1493,.T.);
#11629=ADVANCED_FACE('',(#1904),#1494,.T.);
#11630=ADVANCED_FACE('',(#1905),#1495,.T.);
#11631=ADVANCED_FACE('',(#1906,#1087,#1088,#1089,#1090,#1091,#1092,#1093,
#1094,#1095,#1096,#1097,#1098),#1496,.T.);
#11632=ADVANCED_FACE('',(#1907,#1099,#1100,#1101,#1102,#1103,#1104,#1105,
#1106,#1107,#1108,#1109,#1110),#1497,.F.);
#11633=ADVANCED_FACE('',(#1908),#1498,.T.);
#11634=ADVANCED_FACE('',(#1909),#1499,.T.);
#11635=ADVANCED_FACE('',(#1910),#1500,.T.);
#11636=ADVANCED_FACE('',(#1911),#1501,.T.);
#11637=ADVANCED_FACE('',(#1912),#1502,.T.);
#11638=ADVANCED_FACE('',(#1913),#1503,.F.);
#11639=ADVANCED_FACE('',(#1914),#1504,.T.);
#11640=ADVANCED_FACE('',(#1915),#1505,.T.);
#11641=ADVANCED_FACE('',(#1916),#1506,.T.);
#11642=ADVANCED_FACE('',(#1917),#1507,.T.);
#11643=ADVANCED_FACE('',(#1918),#1508,.T.);
#11644=ADVANCED_FACE('',(#1919),#1509,.F.);
#11645=ADVANCED_FACE('',(#1920),#11279,.F.);
#11646=ADVANCED_FACE('',(#1921),#11280,.F.);
#11647=ADVANCED_FACE('',(#1922),#11281,.F.);
#11648=ADVANCED_FACE('',(#1923),#11282,.F.);
#11649=ADVANCED_FACE('',(#1924),#11283,.F.);
#11650=ADVANCED_FACE('',(#1925),#11284,.F.);
#11651=ADVANCED_FACE('',(#1926),#11285,.F.);
#11652=ADVANCED_FACE('',(#1927),#11286,.F.);
#11653=ADVANCED_FACE('',(#1928,#1111,#1112,#1113,#1114),#1510,.T.);
#11654=ADVANCED_FACE('',(#1929),#1511,.T.);
#11655=ADVANCED_FACE('',(#1930),#1512,.T.);
#11656=ADVANCED_FACE('',(#1931),#1513,.T.);
#11657=ADVANCED_FACE('',(#1932,#1115,#1116,#1117,#1118),#1514,.T.);
#11658=ADVANCED_FACE('',(#1933),#1515,.T.);
#11659=ADVANCED_FACE('',(#1934,#1119,#1120,#1121,#1122),#1516,.T.);
#11660=ADVANCED_FACE('',(#1935),#1517,.T.);
#11661=ADVANCED_FACE('',(#1936),#1518,.T.);
#11662=ADVANCED_FACE('',(#1937,#1123,#1124,#1125,#1126),#1519,.F.);
#11663=ADVANCED_FACE('',(#1938),#11287,.F.);
#11664=ADVANCED_FACE('',(#1939),#11288,.F.);
#11665=ADVANCED_FACE('',(#1940),#11289,.F.);
#11666=ADVANCED_FACE('',(#1941),#11290,.F.);
#11667=ADVANCED_FACE('',(#1942),#11291,.F.);
#11668=ADVANCED_FACE('',(#1943),#11292,.F.);
#11669=ADVANCED_FACE('',(#1944),#11293,.F.);
#11670=ADVANCED_FACE('',(#1945),#11294,.F.);
#11671=ADVANCED_FACE('',(#1946,#1127,#1128,#1129,#1130),#1520,.T.);
#11672=ADVANCED_FACE('',(#1947),#1521,.T.);
#11673=ADVANCED_FACE('',(#1948),#1522,.T.);
#11674=ADVANCED_FACE('',(#1949),#1523,.T.);
#11675=ADVANCED_FACE('',(#1950,#1131,#1132,#1133,#1134),#1524,.T.);
#11676=ADVANCED_FACE('',(#1951),#1525,.T.);
#11677=ADVANCED_FACE('',(#1952,#1135,#1136,#1137,#1138),#1526,.T.);
#11678=ADVANCED_FACE('',(#1953),#1527,.T.);
#11679=ADVANCED_FACE('',(#1954),#1528,.T.);
#11680=ADVANCED_FACE('',(#1955,#1139,#1140,#1141,#1142),#1529,.F.);
#11681=ADVANCED_FACE('',(#1956),#11295,.F.);
#11682=ADVANCED_FACE('',(#1957),#1530,.F.);
#11683=ADVANCED_FACE('',(#1958),#11296,.F.);
#11684=ADVANCED_FACE('',(#1959),#11297,.F.);
#11685=ADVANCED_FACE('',(#1960),#11298,.F.);
#11686=ADVANCED_FACE('',(#1961,#1143,#1144,#1145,#1146),#1531,.T.);
#11687=ADVANCED_FACE('',(#1962,#1147,#1148,#1149,#1150),#1532,.F.);
#11688=ADVANCED_FACE('',(#1963),#11299,.T.);
#11689=ADVANCED_FACE('',(#1964),#11300,.T.);
#11690=ADVANCED_FACE('',(#1965),#11301,.T.);
#11691=ADVANCED_FACE('',(#1966),#1533,.T.);
#11692=ADVANCED_FACE('',(#1967,#1151),#1534,.F.);
#11693=ADVANCED_FACE('',(#1968),#11302,.F.);
#11694=ADVANCED_FACE('',(#1969),#11303,.T.);
#11695=ADVANCED_FACE('',(#1970,#1152),#1535,.T.);
#11696=ADVANCED_FACE('',(#1971,#1153),#1536,.F.);
#11697=ADVANCED_FACE('',(#1972),#11304,.F.);
#11698=ADVANCED_FACE('',(#1973),#11305,.T.);
#11699=ADVANCED_FACE('',(#1974,#1154),#1537,.T.);
#11700=ADVANCED_FACE('',(#1975,#1155),#1538,.F.);
#11701=ADVANCED_FACE('',(#1976),#11306,.F.);
#11702=ADVANCED_FACE('',(#1977),#11307,.T.);
#11703=ADVANCED_FACE('',(#1978,#1156),#1539,.T.);
#11704=ADVANCED_FACE('',(#1979,#1157),#1540,.F.);
#11705=ADVANCED_FACE('',(#1980),#11308,.F.);
#11706=ADVANCED_FACE('',(#1981),#1541,.F.);
#11707=ADVANCED_FACE('',(#1982),#11309,.F.);
#11708=ADVANCED_FACE('',(#1983),#11310,.F.);
#11709=ADVANCED_FACE('',(#1984),#11311,.F.);
#11710=ADVANCED_FACE('',(#1985,#1158,#1159,#1160,#1161),#1542,.T.);
#11711=ADVANCED_FACE('',(#1986,#1162,#1163,#1164,#1165),#1543,.F.);
#11712=ADVANCED_FACE('',(#1987),#11312,.T.);
#11713=ADVANCED_FACE('',(#1988),#11313,.T.);
#11714=ADVANCED_FACE('',(#1989),#11314,.T.);
#11715=ADVANCED_FACE('',(#1990),#1544,.T.);
#11716=ADVANCED_FACE('',(#1991,#1166),#1545,.F.);
#11717=ADVANCED_FACE('',(#1992),#11315,.F.);
#11718=ADVANCED_FACE('',(#1993),#11316,.T.);
#11719=ADVANCED_FACE('',(#1994,#1167),#1546,.T.);
#11720=ADVANCED_FACE('',(#1995,#1168),#1547,.F.);
#11721=ADVANCED_FACE('',(#1996),#11317,.F.);
#11722=ADVANCED_FACE('',(#1997),#11318,.T.);
#11723=ADVANCED_FACE('',(#1998,#1169),#1548,.T.);
#11724=ADVANCED_FACE('',(#1999,#1170),#1549,.F.);
#11725=ADVANCED_FACE('',(#2000),#11319,.F.);
#11726=ADVANCED_FACE('',(#2001),#11320,.T.);
#11727=ADVANCED_FACE('',(#2002,#1171),#1550,.T.);
#11728=ADVANCED_FACE('',(#2003,#1172),#1551,.F.);
#11729=ADVANCED_FACE('',(#2004),#11321,.F.);
#11730=ADVANCED_FACE('',(#2005),#11322,.F.);
#11731=ADVANCED_FACE('',(#2006,#1173),#1552,.T.);
#11732=ADVANCED_FACE('',(#2007,#1174,#1175,#1176,#1177),#1553,.T.);
#11733=ADVANCED_FACE('',(#2008),#11323,.F.);
#11734=ADVANCED_FACE('',(#2009,#1178),#1554,.T.);
#11735=ADVANCED_FACE('',(#2010),#11324,.F.);
#11736=ADVANCED_FACE('',(#2011),#11325,.F.);
#11737=ADVANCED_FACE('',(#2012,#1179),#1555,.T.);
#11738=ADVANCED_FACE('',(#2013),#11326,.F.);
#11739=ADVANCED_FACE('',(#2014),#11327,.F.);
#11740=ADVANCED_FACE('',(#2015),#11328,.F.);
#11741=ADVANCED_FACE('',(#2016),#11329,.F.);
#11742=ADVANCED_FACE('',(#2017),#1556,.T.);
#11743=ADVANCED_FACE('',(#2018),#1557,.T.);
#11744=ADVANCED_FACE('',(#2019,#1180,#1181,#1182,#1183),#1558,.T.);
#11745=ADVANCED_FACE('',(#2020,#1184),#1559,.T.);
#11746=ADVANCED_FACE('',(#2021,#1185,#1186),#1560,.F.);
#11747=ADVANCED_FACE('',(#2022),#11330,.F.);
#11748=ADVANCED_FACE('',(#2023),#11331,.F.);
#11749=ADVANCED_FACE('',(#2024),#11332,.F.);
#11750=ADVANCED_FACE('',(#2025),#11333,.F.);
#11751=ADVANCED_FACE('',(#2026,#1187,#1188,#1189),#1561,.T.);
#11752=ADVANCED_FACE('',(#2027),#11334,.T.);
#11753=ADVANCED_FACE('',(#2028),#11335,.T.);
#11754=ADVANCED_FACE('',(#2029),#11336,.F.);
#11755=ADVANCED_FACE('',(#2030,#1190,#1191,#1192),#1562,.F.);
#11756=ADVANCED_FACE('',(#2031,#1193),#1563,.T.);
#11757=ADVANCED_FACE('',(#2032),#11337,.T.);
#11758=ADVANCED_FACE('',(#2033),#1564,.F.);
#11759=ADVANCED_FACE('',(#2034),#11338,.T.);
#11760=ADVANCED_FACE('',(#2035),#1565,.T.);
#11761=ADVANCED_FACE('',(#2036,#1194),#1566,.T.);
#11762=ADVANCED_FACE('',(#2037),#11339,.T.);
#11763=ADVANCED_FACE('',(#2038),#1567,.F.);
#11764=ADVANCED_FACE('',(#2039),#11340,.T.);
#11765=ADVANCED_FACE('',(#2040),#1568,.T.);
#11766=ADVANCED_FACE('',(#2041),#11341,.F.);
#11767=ADVANCED_FACE('',(#2042),#11342,.F.);
#11768=ADVANCED_FACE('',(#2043),#11343,.F.);
#11769=ADVANCED_FACE('',(#2044),#11344,.F.);
#11770=ADVANCED_FACE('',(#2045,#1195,#1196,#1197),#1569,.T.);
#11771=ADVANCED_FACE('',(#2046),#11345,.T.);
#11772=ADVANCED_FACE('',(#2047),#11346,.T.);
#11773=ADVANCED_FACE('',(#2048),#11347,.F.);
#11774=ADVANCED_FACE('',(#2049,#1198,#1199,#1200),#1570,.F.);
#11775=ADVANCED_FACE('',(#2050,#1201),#1571,.F.);
#11776=ADVANCED_FACE('',(#2051),#11348,.T.);
#11777=ADVANCED_FACE('',(#2052),#1572,.T.);
#11778=ADVANCED_FACE('',(#2053),#11349,.T.);
#11779=ADVANCED_FACE('',(#2054),#1573,.F.);
#11780=ADVANCED_FACE('',(#2055,#1202),#1574,.F.);
#11781=ADVANCED_FACE('',(#2056),#11350,.T.);
#11782=ADVANCED_FACE('',(#2057),#1575,.T.);
#11783=ADVANCED_FACE('',(#2058),#11351,.T.);
#11784=ADVANCED_FACE('',(#2059),#1576,.F.);
#11785=ADVANCED_FACE('',(#2060),#11352,.F.);
#11786=ADVANCED_FACE('',(#2061),#11353,.F.);
#11787=ADVANCED_FACE('',(#2062,#1203),#1577,.T.);
#11788=ADVANCED_FACE('',(#2063,#1204,#1205,#1206,#1207),#1578,.T.);
#11789=ADVANCED_FACE('',(#2064),#11354,.F.);
#11790=ADVANCED_FACE('',(#2065,#1208),#1579,.T.);
#11791=ADVANCED_FACE('',(#2066),#11355,.F.);
#11792=ADVANCED_FACE('',(#2067),#11356,.F.);
#11793=ADVANCED_FACE('',(#2068,#1209),#1580,.T.);
#11794=ADVANCED_FACE('',(#2069),#11357,.F.);
#11795=ADVANCED_FACE('',(#2070),#11358,.F.);
#11796=ADVANCED_FACE('',(#2071),#11359,.F.);
#11797=ADVANCED_FACE('',(#2072),#11360,.F.);
#11798=ADVANCED_FACE('',(#2073),#1581,.T.);
#11799=ADVANCED_FACE('',(#2074),#1582,.T.);
#11800=ADVANCED_FACE('',(#2075,#1210,#1211,#1212,#1213),#1583,.T.);
#11801=ADVANCED_FACE('',(#2076,#1214),#1584,.T.);
#11802=ADVANCED_FACE('',(#2077,#1215,#1216),#1585,.F.);
#11803=ADVANCED_FACE('',(#2078),#11361,.F.);
#11804=ADVANCED_FACE('',(#2079),#11362,.F.);
#11805=ADVANCED_FACE('',(#2080),#11363,.F.);
#11806=ADVANCED_FACE('',(#2081),#11364,.F.);
#11807=ADVANCED_FACE('',(#2082,#1217,#1218,#1219),#1586,.T.);
#11808=ADVANCED_FACE('',(#2083),#11365,.T.);
#11809=ADVANCED_FACE('',(#2084),#11366,.T.);
#11810=ADVANCED_FACE('',(#2085),#11367,.F.);
#11811=ADVANCED_FACE('',(#2086,#1220,#1221,#1222),#1587,.F.);
#11812=ADVANCED_FACE('',(#2087,#1223),#1588,.T.);
#11813=ADVANCED_FACE('',(#2088),#11368,.T.);
#11814=ADVANCED_FACE('',(#2089),#1589,.F.);
#11815=ADVANCED_FACE('',(#2090),#11369,.T.);
#11816=ADVANCED_FACE('',(#2091),#1590,.T.);
#11817=ADVANCED_FACE('',(#2092,#1224),#1591,.T.);
#11818=ADVANCED_FACE('',(#2093),#11370,.T.);
#11819=ADVANCED_FACE('',(#2094),#1592,.F.);
#11820=ADVANCED_FACE('',(#2095),#11371,.T.);
#11821=ADVANCED_FACE('',(#2096),#1593,.T.);
#11822=ADVANCED_FACE('',(#2097),#11372,.F.);
#11823=ADVANCED_FACE('',(#2098),#11373,.F.);
#11824=ADVANCED_FACE('',(#2099),#11374,.F.);
#11825=ADVANCED_FACE('',(#2100),#11375,.F.);
#11826=ADVANCED_FACE('',(#2101,#1225,#1226,#1227),#1594,.T.);
#11827=ADVANCED_FACE('',(#2102),#11376,.T.);
#11828=ADVANCED_FACE('',(#2103),#11377,.T.);
#11829=ADVANCED_FACE('',(#2104),#11378,.F.);
#11830=ADVANCED_FACE('',(#2105,#1228,#1229,#1230),#1595,.F.);
#11831=ADVANCED_FACE('',(#2106,#1231),#1596,.F.);
#11832=ADVANCED_FACE('',(#2107),#11379,.T.);
#11833=ADVANCED_FACE('',(#2108),#1597,.T.);
#11834=ADVANCED_FACE('',(#2109),#11380,.T.);
#11835=ADVANCED_FACE('',(#2110),#1598,.F.);
#11836=ADVANCED_FACE('',(#2111,#1232),#1599,.F.);
#11837=ADVANCED_FACE('',(#2112),#11381,.T.);
#11838=ADVANCED_FACE('',(#2113),#1600,.T.);
#11839=ADVANCED_FACE('',(#2114),#11382,.T.);
#11840=ADVANCED_FACE('',(#2115),#1601,.F.);
#11841=ADVANCED_FACE('',(#2116),#11383,.T.);
#11842=ADVANCED_FACE('',(#2117),#1602,.T.);
#11843=ADVANCED_FACE('',(#2118),#1603,.F.);
#11844=ADVANCED_FACE('',(#2119),#11384,.T.);
#11845=ADVANCED_FACE('',(#2120),#1604,.T.);
#11846=ADVANCED_FACE('',(#2121),#1605,.F.);
#11847=ADVANCED_FACE('',(#2122),#1606,.T.);
#11848=ADVANCED_FACE('',(#2123),#632,.T.);
#11849=ADVANCED_FACE('',(#2124),#11385,.T.);
#11850=ADVANCED_FACE('',(#2125),#633,.T.);
#11851=ADVANCED_FACE('',(#2126,#1233),#1607,.T.);
#11852=ADVANCED_FACE('',(#2127),#634,.T.);
#11853=ADVANCED_FACE('',(#2128),#11386,.T.);
#11854=ADVANCED_FACE('',(#2129),#635,.T.);
#11855=ADVANCED_FACE('',(#2130),#1608,.T.);
#11856=ADVANCED_FACE('',(#2131),#1609,.F.);
#11857=ADVANCED_FACE('',(#2132),#1610,.F.);
#11858=ADVANCED_FACE('',(#2133),#1611,.F.);
#11859=ADVANCED_FACE('',(#2134),#1612,.F.);
#11860=ADVANCED_FACE('',(#2135),#1613,.F.);
#11861=ADVANCED_FACE('',(#2136),#1614,.F.);
#11862=ADVANCED_FACE('',(#2137),#1615,.F.);
#11863=ADVANCED_FACE('',(#2138),#1616,.F.);
#11864=ADVANCED_FACE('',(#2139),#11387,.F.);
#11865=ADVANCED_FACE('',(#2140),#11388,.F.);
#11866=ADVANCED_FACE('',(#2141),#11389,.F.);
#11867=ADVANCED_FACE('',(#2142),#11390,.F.);
#11868=ADVANCED_FACE('',(#2143),#11391,.F.);
#11869=ADVANCED_FACE('',(#2144),#11392,.T.);
#11870=ADVANCED_FACE('',(#2145,#1234,#1235,#1236,#1237,#1238,#1239,#1240,
#1241,#1242,#1243),#1617,.F.);
#11871=ADVANCED_FACE('',(#2146),#1618,.T.);
#11872=ADVANCED_FACE('',(#2147),#11393,.F.);
#11873=ADVANCED_FACE('',(#2148),#11394,.F.);
#11874=ADVANCED_FACE('',(#2149),#11395,.F.);
#11875=ADVANCED_FACE('',(#2150),#11396,.F.);
#11876=ADVANCED_FACE('',(#2151),#11397,.F.);
#11877=ADVANCED_FACE('',(#2152),#11398,.T.);
#11878=ADVANCED_FACE('',(#2153),#1619,.T.);
#11879=ADVANCED_FACE('',(#2154,#1244,#1245,#1246,#1247,#1248,#1249,#1250,
#1251,#1252,#1253),#1620,.T.);
#11880=ADVANCED_FACE('',(#2155),#11399,.F.);
#11881=ADVANCED_FACE('',(#2156),#11400,.F.);
#11882=ADVANCED_FACE('',(#2157),#11401,.F.);
#11883=ADVANCED_FACE('',(#2158),#11402,.F.);
#11884=ADVANCED_FACE('',(#2159),#11403,.F.);
#11885=ADVANCED_FACE('',(#2160),#11404,.T.);
#11886=ADVANCED_FACE('',(#2161,#1254,#1255,#1256,#1257,#1258),#1621,.T.);
#11887=ADVANCED_FACE('',(#2162,#1259,#1260,#1261,#1262,#1263),#1622,.F.);
#11888=ADVANCED_FACE('',(#2163,#1264),#1623,.T.);
#11889=ADVANCED_FACE('',(#2164),#11405,.T.);
#11890=ADVANCED_FACE('',(#2165),#1624,.F.);
#11891=ADVANCED_FACE('',(#2166),#11406,.T.);
#11892=ADVANCED_FACE('',(#2167),#1625,.T.);
#11893=ADVANCED_FACE('',(#2168,#1265),#1626,.T.);
#11894=ADVANCED_FACE('',(#2169),#11407,.T.);
#11895=ADVANCED_FACE('',(#2170),#1627,.F.);
#11896=ADVANCED_FACE('',(#2171),#11408,.T.);
#11897=ADVANCED_FACE('',(#2172),#1628,.T.);
#11898=ADVANCED_FACE('',(#2173,#1266),#1629,.T.);
#11899=ADVANCED_FACE('',(#2174),#11409,.T.);
#11900=ADVANCED_FACE('',(#2175),#1630,.F.);
#11901=ADVANCED_FACE('',(#2176),#11410,.T.);
#11902=ADVANCED_FACE('',(#2177),#1631,.T.);
#11903=ADVANCED_FACE('',(#2178,#1267),#1632,.T.);
#11904=ADVANCED_FACE('',(#2179),#11411,.T.);
#11905=ADVANCED_FACE('',(#2180),#1633,.F.);
#11906=ADVANCED_FACE('',(#2181),#11412,.T.);
#11907=ADVANCED_FACE('',(#2182),#1634,.T.);
#11908=ADVANCED_FACE('',(#2183),#11413,.F.);
#11909=ADVANCED_FACE('',(#2184),#11414,.F.);
#11910=ADVANCED_FACE('',(#2185),#11415,.F.);
#11911=ADVANCED_FACE('',(#2186),#11416,.F.);
#11912=ADVANCED_FACE('',(#2187),#11417,.F.);
#11913=ADVANCED_FACE('',(#2188),#11418,.T.);
#11914=ADVANCED_FACE('',(#2189,#1268,#1269,#1270,#1271,#1272),#1635,.T.);
#11915=ADVANCED_FACE('',(#2190,#1273,#1274,#1275,#1276,#1277),#1636,.F.);
#11916=ADVANCED_FACE('',(#2191,#1278),#1637,.F.);
#11917=ADVANCED_FACE('',(#2192),#11419,.T.);
#11918=ADVANCED_FACE('',(#2193),#1638,.T.);
#11919=ADVANCED_FACE('',(#2194),#11420,.T.);
#11920=ADVANCED_FACE('',(#2195),#1639,.F.);
#11921=ADVANCED_FACE('',(#2196,#1279),#1640,.F.);
#11922=ADVANCED_FACE('',(#2197),#11421,.T.);
#11923=ADVANCED_FACE('',(#2198),#1641,.T.);
#11924=ADVANCED_FACE('',(#2199),#11422,.T.);
#11925=ADVANCED_FACE('',(#2200),#1642,.F.);
#11926=ADVANCED_FACE('',(#2201,#1280),#1643,.F.);
#11927=ADVANCED_FACE('',(#2202),#11423,.T.);
#11928=ADVANCED_FACE('',(#2203),#1644,.T.);
#11929=ADVANCED_FACE('',(#2204),#11424,.T.);
#11930=ADVANCED_FACE('',(#2205),#1645,.F.);
#11931=ADVANCED_FACE('',(#2206,#1281),#1646,.F.);
#11932=ADVANCED_FACE('',(#2207),#11425,.T.);
#11933=ADVANCED_FACE('',(#2208),#1647,.T.);
#11934=ADVANCED_FACE('',(#2209),#11426,.T.);
#11935=ADVANCED_FACE('',(#2210),#1648,.F.);
#11936=ADVANCED_FACE('',(#2211),#11427,.F.);
#11937=ADVANCED_FACE('',(#2212),#11428,.F.);
#11938=ADVANCED_FACE('',(#2213),#11429,.F.);
#11939=ADVANCED_FACE('',(#2214),#11430,.F.);
#11940=ADVANCED_FACE('',(#2215),#11431,.F.);
#11941=ADVANCED_FACE('',(#2216),#11432,.T.);
#11942=ADVANCED_FACE('',(#2217,#1282,#1283,#1284,#1285,#1286),#1649,.T.);
#11943=ADVANCED_FACE('',(#2218,#1287,#1288,#1289,#1290,#1291),#1650,.F.);
#11944=ADVANCED_FACE('',(#2219,#1292),#1651,.T.);
#11945=ADVANCED_FACE('',(#2220),#11433,.T.);
#11946=ADVANCED_FACE('',(#2221),#1652,.F.);
#11947=ADVANCED_FACE('',(#2222),#11434,.T.);
#11948=ADVANCED_FACE('',(#2223),#1653,.T.);
#11949=ADVANCED_FACE('',(#2224,#1293),#1654,.T.);
#11950=ADVANCED_FACE('',(#2225),#11435,.T.);
#11951=ADVANCED_FACE('',(#2226),#1655,.F.);
#11952=ADVANCED_FACE('',(#2227),#11436,.T.);
#11953=ADVANCED_FACE('',(#2228),#1656,.T.);
#11954=ADVANCED_FACE('',(#2229,#1294),#1657,.T.);
#11955=ADVANCED_FACE('',(#2230),#11437,.T.);
#11956=ADVANCED_FACE('',(#2231),#1658,.F.);
#11957=ADVANCED_FACE('',(#2232),#11438,.T.);
#11958=ADVANCED_FACE('',(#2233),#1659,.T.);
#11959=ADVANCED_FACE('',(#2234,#1295),#1660,.T.);
#11960=ADVANCED_FACE('',(#2235),#11439,.T.);
#11961=ADVANCED_FACE('',(#2236),#1661,.F.);
#11962=ADVANCED_FACE('',(#2237),#11440,.T.);
#11963=ADVANCED_FACE('',(#2238),#1662,.T.);
#11964=ADVANCED_FACE('',(#2239),#11441,.F.);
#11965=ADVANCED_FACE('',(#2240),#11442,.F.);
#11966=ADVANCED_FACE('',(#2241),#11443,.F.);
#11967=ADVANCED_FACE('',(#2242),#11444,.F.);
#11968=ADVANCED_FACE('',(#2243),#11445,.F.);
#11969=ADVANCED_FACE('',(#2244),#11446,.T.);
#11970=ADVANCED_FACE('',(#2245,#1296,#1297,#1298,#1299,#1300),#1663,.T.);
#11971=ADVANCED_FACE('',(#2246,#1301,#1302,#1303,#1304,#1305),#1664,.F.);
#11972=ADVANCED_FACE('',(#2247,#1306),#1665,.F.);
#11973=ADVANCED_FACE('',(#2248),#11447,.T.);
#11974=ADVANCED_FACE('',(#2249),#1666,.T.);
#11975=ADVANCED_FACE('',(#2250),#11448,.T.);
#11976=ADVANCED_FACE('',(#2251),#1667,.F.);
#11977=ADVANCED_FACE('',(#2252,#1307),#1668,.F.);
#11978=ADVANCED_FACE('',(#2253),#11449,.T.);
#11979=ADVANCED_FACE('',(#2254),#1669,.T.);
#11980=ADVANCED_FACE('',(#2255),#11450,.T.);
#11981=ADVANCED_FACE('',(#2256),#1670,.F.);
#11982=ADVANCED_FACE('',(#2257,#1308),#1671,.F.);
#11983=ADVANCED_FACE('',(#2258),#11451,.T.);
#11984=ADVANCED_FACE('',(#2259),#1672,.T.);
#11985=ADVANCED_FACE('',(#2260),#11452,.T.);
#11986=ADVANCED_FACE('',(#2261),#1673,.F.);
#11987=ADVANCED_FACE('',(#2262,#1309),#1674,.F.);
#11988=ADVANCED_FACE('',(#2263),#11453,.T.);
#11989=ADVANCED_FACE('',(#2264),#1675,.T.);
#11990=ADVANCED_FACE('',(#2265),#11454,.T.);
#11991=ADVANCED_FACE('',(#2266),#1676,.F.);
#11992=ADVANCED_FACE('',(#2267),#11455,.F.);
#11993=ADVANCED_FACE('',(#2268),#11456,.F.);
#11994=ADVANCED_FACE('',(#2269),#11457,.F.);
#11995=ADVANCED_FACE('',(#2270),#11458,.F.);
#11996=ADVANCED_FACE('',(#2271),#11459,.F.);
#11997=ADVANCED_FACE('',(#2272),#11460,.T.);
#11998=ADVANCED_FACE('',(#2273),#1677,.T.);
#11999=ADVANCED_FACE('',(#2274,#1310,#1311,#1312,#1313,#1314,#1315,#1316,
#1317,#1318,#1319),#1678,.T.);
#12000=ADVANCED_FACE('',(#2275),#11461,.F.);
#12001=ADVANCED_FACE('',(#2276),#11462,.F.);
#12002=ADVANCED_FACE('',(#2277),#11463,.F.);
#12003=ADVANCED_FACE('',(#2278),#11464,.F.);
#12004=ADVANCED_FACE('',(#2279),#11465,.F.);
#12005=ADVANCED_FACE('',(#2280),#11466,.T.);
#12006=ADVANCED_FACE('',(#2281),#1679,.T.);
#12007=ADVANCED_FACE('',(#2282,#1320,#1321,#1322,#1323,#1324,#1325,#1326,
#1327,#1328,#1329),#1680,.F.);
#12008=ADVANCED_FACE('',(#2283),#11467,.F.);
#12009=ADVANCED_FACE('',(#2284),#11468,.F.);
#12010=ADVANCED_FACE('',(#2285),#11469,.F.);
#12011=ADVANCED_FACE('',(#2286),#11470,.F.);
#12012=ADVANCED_FACE('',(#2287),#11471,.F.);
#12013=ADVANCED_FACE('',(#2288),#11472,.T.);
#12014=ADVANCED_FACE('',(#2289,#1330,#1331,#1332,#1333,#1334),#1681,.T.);
#12015=ADVANCED_FACE('',(#2290,#1335,#1336,#1337,#1338,#1339),#1682,.F.);
#12016=ADVANCED_FACE('',(#2291,#1340),#1683,.T.);
#12017=ADVANCED_FACE('',(#2292),#11473,.T.);
#12018=ADVANCED_FACE('',(#2293),#1684,.F.);
#12019=ADVANCED_FACE('',(#2294),#11474,.T.);
#12020=ADVANCED_FACE('',(#2295),#1685,.T.);
#12021=ADVANCED_FACE('',(#2296,#1341),#1686,.T.);
#12022=ADVANCED_FACE('',(#2297),#11475,.T.);
#12023=ADVANCED_FACE('',(#2298),#1687,.F.);
#12024=ADVANCED_FACE('',(#2299),#11476,.T.);
#12025=ADVANCED_FACE('',(#2300),#1688,.T.);
#12026=ADVANCED_FACE('',(#2301,#1342),#1689,.T.);
#12027=ADVANCED_FACE('',(#2302),#11477,.T.);
#12028=ADVANCED_FACE('',(#2303),#1690,.F.);
#12029=ADVANCED_FACE('',(#2304),#11478,.T.);
#12030=ADVANCED_FACE('',(#2305),#1691,.T.);
#12031=ADVANCED_FACE('',(#2306,#1343),#1692,.T.);
#12032=ADVANCED_FACE('',(#2307),#11479,.T.);
#12033=ADVANCED_FACE('',(#2308),#1693,.F.);
#12034=ADVANCED_FACE('',(#2309),#11480,.T.);
#12035=ADVANCED_FACE('',(#2310),#1694,.T.);
#12036=ADVANCED_FACE('',(#2311),#11481,.F.);
#12037=ADVANCED_FACE('',(#2312),#11482,.F.);
#12038=ADVANCED_FACE('',(#2313),#11483,.F.);
#12039=ADVANCED_FACE('',(#2314),#11484,.F.);
#12040=ADVANCED_FACE('',(#2315),#11485,.F.);
#12041=ADVANCED_FACE('',(#2316),#11486,.T.);
#12042=ADVANCED_FACE('',(#2317,#1344,#1345,#1346,#1347,#1348),#1695,.T.);
#12043=ADVANCED_FACE('',(#2318,#1349,#1350,#1351,#1352,#1353),#1696,.F.);
#12044=ADVANCED_FACE('',(#2319,#1354),#1697,.F.);
#12045=ADVANCED_FACE('',(#2320),#11487,.T.);
#12046=ADVANCED_FACE('',(#2321),#1698,.T.);
#12047=ADVANCED_FACE('',(#2322),#11488,.T.);
#12048=ADVANCED_FACE('',(#2323),#1699,.F.);
#12049=ADVANCED_FACE('',(#2324,#1355),#1700,.F.);
#12050=ADVANCED_FACE('',(#2325),#11489,.T.);
#12051=ADVANCED_FACE('',(#2326),#1701,.T.);
#12052=ADVANCED_FACE('',(#2327),#11490,.T.);
#12053=ADVANCED_FACE('',(#2328),#1702,.F.);
#12054=ADVANCED_FACE('',(#2329,#1356),#1703,.F.);
#12055=ADVANCED_FACE('',(#2330),#11491,.T.);
#12056=ADVANCED_FACE('',(#2331),#1704,.T.);
#12057=ADVANCED_FACE('',(#2332),#11492,.T.);
#12058=ADVANCED_FACE('',(#2333),#1705,.F.);
#12059=ADVANCED_FACE('',(#2334,#1357),#1706,.F.);
#12060=ADVANCED_FACE('',(#2335),#11493,.T.);
#12061=ADVANCED_FACE('',(#2336),#1707,.T.);
#12062=ADVANCED_FACE('',(#2337),#11494,.T.);
#12063=ADVANCED_FACE('',(#2338),#1708,.F.);
#12064=ADVANCED_FACE('',(#2339),#11495,.F.);
#12065=ADVANCED_FACE('',(#2340),#11496,.F.);
#12066=ADVANCED_FACE('',(#2341),#11497,.F.);
#12067=ADVANCED_FACE('',(#2342),#11498,.F.);
#12068=ADVANCED_FACE('',(#2343),#11499,.F.);
#12069=ADVANCED_FACE('',(#2344),#11500,.T.);
#12070=ADVANCED_FACE('',(#2345,#1358,#1359,#1360,#1361,#1362),#1709,.T.);
#12071=ADVANCED_FACE('',(#2346,#1363,#1364,#1365,#1366,#1367),#1710,.F.);
#12072=ADVANCED_FACE('',(#2347,#1368),#1711,.T.);
#12073=ADVANCED_FACE('',(#2348),#11501,.T.);
#12074=ADVANCED_FACE('',(#2349),#1712,.F.);
#12075=ADVANCED_FACE('',(#2350),#11502,.T.);
#12076=ADVANCED_FACE('',(#2351),#1713,.T.);
#12077=ADVANCED_FACE('',(#2352,#1369),#1714,.T.);
#12078=ADVANCED_FACE('',(#2353),#11503,.T.);
#12079=ADVANCED_FACE('',(#2354),#1715,.F.);
#12080=ADVANCED_FACE('',(#2355),#11504,.T.);
#12081=ADVANCED_FACE('',(#2356),#1716,.T.);
#12082=ADVANCED_FACE('',(#2357,#1370),#1717,.T.);
#12083=ADVANCED_FACE('',(#2358),#11505,.T.);
#12084=ADVANCED_FACE('',(#2359),#1718,.F.);
#12085=ADVANCED_FACE('',(#2360),#11506,.T.);
#12086=ADVANCED_FACE('',(#2361),#1719,.T.);
#12087=ADVANCED_FACE('',(#2362,#1371),#1720,.T.);
#12088=ADVANCED_FACE('',(#2363),#11507,.T.);
#12089=ADVANCED_FACE('',(#2364),#1721,.F.);
#12090=ADVANCED_FACE('',(#2365),#11508,.T.);
#12091=ADVANCED_FACE('',(#2366),#1722,.T.);
#12092=ADVANCED_FACE('',(#2367),#11509,.F.);
#12093=ADVANCED_FACE('',(#2368),#11510,.F.);
#12094=ADVANCED_FACE('',(#2369),#11511,.F.);
#12095=ADVANCED_FACE('',(#2370),#11512,.F.);
#12096=ADVANCED_FACE('',(#2371),#11513,.F.);
#12097=ADVANCED_FACE('',(#2372),#11514,.T.);
#12098=ADVANCED_FACE('',(#2373,#1372,#1373,#1374,#1375,#1376),#1723,.T.);
#12099=ADVANCED_FACE('',(#2374,#1377,#1378,#1379,#1380,#1381),#1724,.F.);
#12100=ADVANCED_FACE('',(#2375,#1382),#1725,.F.);
#12101=ADVANCED_FACE('',(#2376),#11515,.T.);
#12102=ADVANCED_FACE('',(#2377),#1726,.T.);
#12103=ADVANCED_FACE('',(#2378),#11516,.T.);
#12104=ADVANCED_FACE('',(#2379),#1727,.F.);
#12105=ADVANCED_FACE('',(#2380,#1383),#1728,.F.);
#12106=ADVANCED_FACE('',(#2381),#11517,.T.);
#12107=ADVANCED_FACE('',(#2382),#1729,.T.);
#12108=ADVANCED_FACE('',(#2383),#11518,.T.);
#12109=ADVANCED_FACE('',(#2384),#1730,.F.);
#12110=ADVANCED_FACE('',(#2385,#1384),#1731,.F.);
#12111=ADVANCED_FACE('',(#2386),#11519,.T.);
#12112=ADVANCED_FACE('',(#2387),#1732,.T.);
#12113=ADVANCED_FACE('',(#2388),#11520,.T.);
#12114=ADVANCED_FACE('',(#2389),#1733,.F.);
#12115=ADVANCED_FACE('',(#2390,#1385),#1734,.F.);
#12116=ADVANCED_FACE('',(#2391),#11521,.T.);
#12117=ADVANCED_FACE('',(#2392),#1735,.T.);
#12118=ADVANCED_FACE('',(#2393),#11522,.T.);
#12119=ADVANCED_FACE('',(#2394),#1736,.F.);
#12120=ADVANCED_FACE('',(#2395),#627,.F.);
#12121=ADVANCED_FACE('',(#2396),#11523,.T.);
#12122=ADVANCED_FACE('',(#2397),#11524,.F.);
#12123=ADVANCED_FACE('',(#2398),#636,.F.);
#12124=ADVANCED_FACE('',(#2399,#1386),#1737,.T.);
#12125=ADVANCED_FACE('',(#2400),#11525,.T.);
#12126=ADVANCED_FACE('',(#2401,#1387),#1738,.T.);
#12127=ADVANCED_FACE('',(#2402),#637,.F.);
#12128=ADVANCED_FACE('',(#2403),#628,.F.);
#12129=ADVANCED_FACE('',(#2404),#11526,.F.);
#12130=ADVANCED_FACE('',(#2405,#1388),#1739,.T.);
#12131=ADVANCED_FACE('',(#2406),#638,.T.);
#12132=ADVANCED_FACE('',(#2407),#11527,.T.);
#12133=ADVANCED_FACE('',(#2408),#639,.T.);
#12134=ADVANCED_FACE('',(#2409,#1389),#1740,.T.);
#12135=ADVANCED_FACE('',(#2410),#11528,.F.);
#12136=ADVANCED_FACE('',(#2411),#613,.T.);
#12137=ADVANCED_FACE('',(#2412),#614,.T.);
#12138=ADVANCED_FACE('',(#2413),#615,.T.);
#12139=ADVANCED_FACE('',(#2414),#616,.T.);
#12140=ADVANCED_FACE('',(#2415),#617,.T.);
#12141=ADVANCED_FACE('',(#2416),#618,.T.);
#12142=ADVANCED_FACE('',(#2417),#619,.T.);
#12143=ADVANCED_FACE('',(#2418),#620,.F.);
#12144=ADVANCED_FACE('',(#2419),#11529,.T.);
#12145=ADVANCED_FACE('',(#2420),#1741,.T.);
#12146=ADVANCED_FACE('',(#2421),#621,.F.);
#12147=ADVANCED_FACE('',(#2422),#1742,.T.);
#12148=ADVANCED_FACE('',(#2423),#622,.F.);
#12149=ADVANCED_FACE('',(#2424),#1743,.T.);
#12150=ADVANCED_FACE('',(#2425),#623,.F.);
#12151=ADVANCED_FACE('',(#2426),#1744,.T.);
#12152=ADVANCED_FACE('',(#2427),#624,.F.);
#12153=ADVANCED_FACE('',(#2428),#1745,.T.);
#12154=ADVANCED_FACE('',(#2429),#625,.F.);
#12155=ADVANCED_FACE('',(#2430),#11530,.F.);
#12156=ADVANCED_FACE('',(#2431),#1746,.T.);
#12157=ADVANCED_FACE('',(#2432),#626,.F.);
#12158=ADVANCED_FACE('',(#2433,#1390),#1747,.T.);
#12159=ADVANCED_FACE('',(#2434),#1748,.T.);
#12160=ADVANCED_FACE('',(#2435,#1391),#1749,.T.);
#12161=ADVANCED_FACE('',(#2436),#11531,.T.);
#12162=ADVANCED_FACE('',(#2437,#1392),#1750,.T.);
#12163=ADVANCED_FACE('',(#2438),#11532,.F.);
#12164=ADVANCED_FACE('',(#2439,#1393),#1751,.T.);
#12165=ADVANCED_FACE('',(#2440),#11533,.T.);
#12166=ADVANCED_FACE('',(#2441,#1394),#1752,.T.);
#12167=ADVANCED_FACE('',(#2442),#11534,.F.);
#12168=ADVANCED_FACE('',(#2443),#11535,.F.);
#12169=ADVANCED_FACE('',(#2444),#11536,.F.);
#12170=ADVANCED_FACE('',(#2445),#11537,.F.);
#12171=ADVANCED_FACE('',(#2446),#11538,.F.);
#12172=ADVANCED_FACE('',(#2447),#11539,.F.);
#12173=ADVANCED_FACE('',(#2448),#11540,.F.);
#12174=ADVANCED_FACE('',(#2449),#11541,.F.);
#12175=ADVANCED_FACE('',(#2450),#11542,.F.);
#12176=ADVANCED_FACE('',(#2451),#1753,.T.);
#12177=ADVANCED_FACE('',(#2452),#1754,.T.);
#12178=ADVANCED_FACE('',(#2453),#1755,.T.);
#12179=ADVANCED_FACE('',(#2454),#11543,.T.);
#12180=ADVANCED_FACE('',(#2455),#11544,.T.);
#12181=ADVANCED_FACE('',(#2456,#1395,#1396,#1397,#1398,#1399,#1400,#1401,
#1402),#1756,.F.);
#12182=ADVANCED_FACE('',(#2457),#1757,.T.);
#12183=ADVANCED_FACE('',(#2458),#1758,.T.);
#12184=ADVANCED_FACE('',(#2459),#1759,.T.);
#12185=ADVANCED_FACE('',(#2460),#1760,.T.);
#12186=ADVANCED_FACE('',(#2461),#11545,.T.);
#12187=ADVANCED_FACE('',(#2462),#1761,.T.);
#12188=ADVANCED_FACE('',(#2463,#1403,#1404,#1405,#1406,#1407,#1408,#1409,
#1410),#1762,.T.);
#12189=ADVANCED_FACE('',(#2464),#1763,.T.);
#12190=ADVANCED_FACE('',(#2465),#1764,.T.);
#12191=ADVANCED_FACE('',(#2466),#1765,.T.);
#12192=ADVANCED_FACE('',(#2467),#1766,.T.);
#12193=ADVANCED_FACE('',(#2468),#1767,.T.);
#12194=ADVANCED_FACE('',(#2469),#1768,.F.);
#12195=ADVANCED_FACE('',(#2470),#1769,.T.);
#12196=ADVANCED_FACE('',(#2471),#1770,.T.);
#12197=ADVANCED_FACE('',(#2472),#1771,.T.);
#12198=ADVANCED_FACE('',(#2473),#1772,.T.);
#12199=ADVANCED_FACE('',(#2474),#1773,.T.);
#12200=ADVANCED_FACE('',(#2475),#1774,.F.);
#12201=ADVANCED_FACE('',(#2476),#1775,.T.);
#12202=ADVANCED_FACE('',(#2477),#1776,.T.);
#12203=ADVANCED_FACE('',(#2478),#1777,.T.);
#12204=ADVANCED_FACE('',(#2479),#1778,.T.);
#12205=ADVANCED_FACE('',(#2480),#1779,.T.);
#12206=ADVANCED_FACE('',(#2481),#1780,.F.);
#12207=ADVANCED_FACE('',(#2482),#11546,.F.);
#12208=ADVANCED_FACE('',(#2483),#1781,.F.);
#12209=ADVANCED_FACE('',(#2484),#11547,.F.);
#12210=ADVANCED_FACE('',(#2485),#11548,.F.);
#12211=ADVANCED_FACE('',(#2486),#11549,.F.);
#12212=ADVANCED_FACE('',(#2487,#1411,#1412,#1413,#1414),#1782,.T.);
#12213=ADVANCED_FACE('',(#2488,#1415,#1416,#1417,#1418),#1783,.F.);
#12214=ADVANCED_FACE('',(#2489),#11550,.T.);
#12215=ADVANCED_FACE('',(#2490),#11551,.T.);
#12216=ADVANCED_FACE('',(#2491),#11552,.T.);
#12217=ADVANCED_FACE('',(#2492),#1784,.T.);
#12218=ADVANCED_FACE('',(#2493,#1419),#1785,.F.);
#12219=ADVANCED_FACE('',(#2494),#11553,.F.);
#12220=ADVANCED_FACE('',(#2495),#11554,.T.);
#12221=ADVANCED_FACE('',(#2496,#1420),#1786,.T.);
#12222=ADVANCED_FACE('',(#2497,#1421),#1787,.F.);
#12223=ADVANCED_FACE('',(#2498),#11555,.F.);
#12224=ADVANCED_FACE('',(#2499),#11556,.T.);
#12225=ADVANCED_FACE('',(#2500,#1422),#1788,.T.);
#12226=ADVANCED_FACE('',(#2501,#1423),#1789,.F.);
#12227=ADVANCED_FACE('',(#2502),#11557,.F.);
#12228=ADVANCED_FACE('',(#2503),#11558,.T.);
#12229=ADVANCED_FACE('',(#2504,#1424),#1790,.T.);
#12230=ADVANCED_FACE('',(#2505,#1425),#1791,.F.);
#12231=ADVANCED_FACE('',(#2506),#11559,.F.);
#12232=ADVANCED_FACE('',(#2507),#11560,.T.);
#12233=ADVANCED_FACE('',(#2508,#1426),#1792,.T.);
#12234=ADVANCED_FACE('',(#2509,#1427),#1793,.F.);
#12235=ADVANCED_FACE('',(#2510),#11561,.F.);
#12236=ADVANCED_FACE('',(#2511),#1794,.F.);
#12237=ADVANCED_FACE('',(#2512),#11562,.F.);
#12238=ADVANCED_FACE('',(#2513),#11563,.F.);
#12239=ADVANCED_FACE('',(#2514),#11564,.F.);
#12240=ADVANCED_FACE('',(#2515,#1428,#1429,#1430,#1431),#1795,.T.);
#12241=ADVANCED_FACE('',(#2516,#1432,#1433,#1434,#1435),#1796,.F.);
#12242=ADVANCED_FACE('',(#2517),#11565,.T.);
#12243=ADVANCED_FACE('',(#2518),#11566,.T.);
#12244=ADVANCED_FACE('',(#2519),#11567,.T.);
#12245=ADVANCED_FACE('',(#2520),#1797,.T.);
#12246=ADVANCED_FACE('',(#2521,#1436),#1798,.F.);
#12247=ADVANCED_FACE('',(#2522),#11568,.F.);
#12248=ADVANCED_FACE('',(#2523),#11569,.T.);
#12249=ADVANCED_FACE('',(#2524,#1437),#1799,.T.);
#12250=ADVANCED_FACE('',(#2525,#1438),#1800,.F.);
#12251=ADVANCED_FACE('',(#2526),#11570,.F.);
#12252=ADVANCED_FACE('',(#2527),#11571,.T.);
#12253=ADVANCED_FACE('',(#2528,#1439),#1801,.T.);
#12254=ADVANCED_FACE('',(#2529,#1440),#1802,.F.);
#12255=ADVANCED_FACE('',(#2530),#11572,.F.);
#12256=ADVANCED_FACE('',(#2531),#11573,.T.);
#12257=ADVANCED_FACE('',(#2532,#1441),#1803,.T.);
#12258=ADVANCED_FACE('',(#2533,#1442),#1804,.F.);
#12259=ADVANCED_FACE('',(#2534),#1805,.T.);
#12260=ADVANCED_FACE('',(#2535),#640,.T.);
#12261=ADVANCED_FACE('',(#2536),#11574,.T.);
#12262=ADVANCED_FACE('',(#2537),#641,.T.);
#12263=ADVANCED_FACE('',(#2538,#1443),#1806,.T.);
#12264=ADVANCED_FACE('',(#2539),#642,.T.);
#12265=ADVANCED_FACE('',(#2540),#11575,.T.);
#12266=ADVANCED_FACE('',(#2541),#643,.T.);
#12267=ADVANCED_FACE('',(#2542),#1807,.T.);
#12268=ADVANCED_FACE('',(#2543),#1808,.F.);
#12269=ADVANCED_FACE('',(#2544),#1809,.F.);
#12270=ADVANCED_FACE('',(#2545),#1810,.F.);
#12271=ADVANCED_FACE('',(#2546),#1811,.F.);
#12272=ADVANCED_FACE('',(#2547),#1812,.F.);
#12273=ADVANCED_FACE('',(#2548),#1813,.F.);
#12274=ADVANCED_FACE('',(#2549),#1814,.F.);
#12275=ADVANCED_FACE('',(#2550),#1815,.F.);
#12276=ADVANCED_FACE('',(#2551),#11576,.F.);
#12277=ADVANCED_FACE('',(#2552),#11577,.F.);
#12278=ADVANCED_FACE('',(#2553),#11578,.F.);
#12279=ADVANCED_FACE('',(#2554),#1816,.T.);
#12280=ADVANCED_FACE('',(#2555,#1444,#1445,#1446),#1817,.T.);
#12281=ADVANCED_FACE('',(#2556),#1818,.T.);
#12282=ADVANCED_FACE('',(#2557,#1447,#1448,#1449),#1819,.T.);
#12283=ADVANCED_FACE('',(#2558),#1820,.T.);
#12284=ADVANCED_FACE('',(#2559),#1821,.F.);
#12285=ADVANCED_FACE('',(#2560),#11579,.F.);
#12286=ADVANCED_FACE('',(#2561),#11580,.F.);
#12287=ADVANCED_FACE('',(#2562),#11581,.F.);
#12288=ADVANCED_FACE('',(#2563),#1822,.T.);
#12289=ADVANCED_FACE('',(#2564),#1823,.T.);
#12290=ADVANCED_FACE('',(#2565),#1824,.T.);
#12291=ADVANCED_FACE('',(#2566),#1825,.T.);
#12292=ADVANCED_FACE('',(#2567,#1450,#1451,#1452),#1826,.T.);
#12293=ADVANCED_FACE('',(#2568,#1453,#1454,#1455),#1827,.F.);
#12294=ADVANCED_FACE('',(#2569),#11582,.F.);
#12295=ADVANCED_FACE('',(#2570),#11583,.F.);
#12296=ADVANCED_FACE('',(#2571),#11584,.F.);
#12297=ADVANCED_FACE('',(#2572),#1828,.T.);
#12298=ADVANCED_FACE('',(#2573),#1829,.T.);
#12299=ADVANCED_FACE('',(#2574),#1830,.T.);
#12300=ADVANCED_FACE('',(#2575),#1831,.T.);
#12301=ADVANCED_FACE('',(#2576,#1456,#1457,#1458),#1832,.T.);
#12302=ADVANCED_FACE('',(#2577,#1459,#1460,#1461),#1833,.F.);
#12303=ADVANCED_FACE('',(#2578),#11585,.F.);
#12304=ADVANCED_FACE('',(#2579,#1462),#1834,.T.);
#12305=ADVANCED_FACE('',(#2580),#1835,.T.);
#12306=ADVANCED_FACE('',(#2581,#1463),#1836,.T.);
#12307=ADVANCED_FACE('',(#2582),#1837,.T.);
#12308=ADVANCED_FACE('',(#2583),#1838,.T.);
#12309=ADVANCED_FACE('',(#2584),#1839,.F.);
#12310=ADVANCED_FACE('',(#2585),#11586,.F.);
#12311=ADVANCED_FACE('',(#2586),#1840,.T.);
#12312=ADVANCED_FACE('',(#2587,#1464),#1841,.T.);
#12313=ADVANCED_FACE('',(#2588),#11587,.T.);
#12314=ADVANCED_FACE('',(#2589),#1842,.F.);
#12315=ADVANCED_FACE('',(#2590),#11588,.T.);
#12316=ADVANCED_FACE('',(#2591,#1465),#1843,.T.);
#12317=ADVANCED_FACE('',(#2592),#11589,.F.);
#12318=ADVANCED_FACE('',(#2593),#11590,.T.);
#12319=ADVANCED_FACE('',(#2594,#1466),#1844,.T.);
#12320=ADVANCED_FACE('',(#2595,#1467),#1845,.F.);
#12321=ADVANCED_FACE('',(#2596),#11591,.F.);
#12322=ADVANCED_FACE('',(#2597),#11592,.T.);
#12323=ADVANCED_FACE('',(#2598,#1468),#1846,.T.);
#12324=ADVANCED_FACE('',(#2599,#1469),#1847,.F.);
#12325=ADVANCED_FACE('',(#2600),#1848,.F.);
#12326=ADVANCED_FACE('',(#2601),#1849,.F.);
#12327=ADVANCED_FACE('',(#2602),#1850,.F.);
#12328=ADVANCED_FACE('',(#2603),#1851,.F.);
#12329=ADVANCED_FACE('',(#2604),#1852,.F.);
#12330=ADVANCED_FACE('',(#2605,#1470),#1853,.T.);
#12331=ADVANCED_FACE('',(#2606),#11593,.T.);
#12332=ADVANCED_FACE('',(#2607,#1471),#1854,.T.);
#12333=ADVANCED_FACE('',(#2608),#11594,.T.);
#12334=ADVANCED_FACE('',(#2609,#1472),#1855,.T.);
#12335=ADVANCED_FACE('',(#2610),#11595,.T.);
#12336=ADVANCED_FACE('',(#2611,#1473),#1856,.T.);
#12337=ADVANCED_FACE('',(#2612),#11596,.T.);
#12338=ADVANCED_FACE('',(#2613,#1474),#1857,.T.);
#12339=ADVANCED_FACE('',(#2614),#11597,.T.);
#12340=ADVANCED_FACE('',(#2615,#1475),#1858,.T.);
#12341=ADVANCED_FACE('',(#2616,#1476),#11598,.F.);
#12342=ADVANCED_FACE('',(#2617),#1859,.F.);
#12343=ADVANCED_FACE('',(#2618),#1860,.F.);
#12344=ADVANCED_FACE('',(#2619),#1861,.F.);
#12345=ADVANCED_FACE('',(#2620),#1862,.F.);
#12346=ADVANCED_FACE('',(#2621,#1477),#1863,.T.);
#12347=ADVANCED_FACE('',(#2622,#1478),#11599,.T.);
#12348=ADVANCED_FACE('',(#2623,#1479),#1864,.T.);
#12349=ADVANCED_FACE('',(#2624,#1480),#11600,.F.);
#12350=ADVANCED_FACE('',(#2625),#1865,.F.);
#12351=ADVANCED_FACE('',(#2626),#1866,.F.);
#12352=ADVANCED_FACE('',(#2627),#1867,.F.);
#12353=ADVANCED_FACE('',(#2628),#1868,.F.);
#12354=ADVANCED_FACE('',(#2629),#1869,.F.);
#12355=ADVANCED_FACE('',(#2630),#1870,.F.);
#12356=ADVANCED_FACE('',(#2631),#1871,.F.);
#12357=ADVANCED_FACE('',(#2632),#1872,.F.);
#12358=ADVANCED_FACE('',(#2633),#1873,.F.);
#12359=ADVANCED_FACE('',(#2634),#1874,.T.);
#12360=ADVANCED_FACE('',(#2635),#644,.T.);
#12361=ADVANCED_FACE('',(#2636),#11601,.T.);
#12362=ADVANCED_FACE('',(#2637),#645,.T.);
#12363=ADVANCED_FACE('',(#2638,#1481),#1875,.T.);
#12364=ADVANCED_FACE('',(#2639),#646,.T.);
#12365=ADVANCED_FACE('',(#2640),#11602,.T.);
#12366=ADVANCED_FACE('',(#2641),#11603,.F.);
#12367=ADVANCED_FACE('',(#2642),#11604,.T.);
#12368=ADVANCED_FACE('',(#2643,#1482,#1483),#1876,.F.);
#12369=ADVANCED_FACE('',(#2644),#1877,.T.);
#12370=ADVANCED_FACE('',(#2645),#11605,.F.);
#12371=ADVANCED_FACE('',(#2646),#11606,.T.);
#12372=ADVANCED_FACE('',(#2647),#1878,.T.);
#12373=ADVANCED_FACE('',(#2648,#1484,#1485),#1879,.T.);
#12374=ADVANCED_FACE('',(#2649),#11607,.T.);
#12375=ADVANCED_FACE('',(#2650),#1880,.T.);
#12376=ADVANCED_FACE('',(#2651),#1881,.F.);
#12377=ADVANCED_FACE('',(#2652),#11608,.F.);
#12378=ADVANCED_FACE('',(#2653),#11609,.T.);
#12379=ADVANCED_FACE('',(#2654,#1486),#1882,.T.);
#12380=ADVANCED_FACE('',(#2655,#1487),#1883,.F.);
#12381=ADVANCED_FACE('',(#2656),#11610,.F.);
#12382=ADVANCED_FACE('',(#2657),#11611,.T.);
#12383=ADVANCED_FACE('',(#2658,#1488),#1884,.T.);
#12384=ADVANCED_FACE('',(#2659,#1489),#1885,.F.);
#12385=ADVANCED_FACE('',(#2660),#11612,.F.);
#12386=ADVANCED_FACE('',(#2661),#11613,.T.);
#12387=ADVANCED_FACE('',(#2662,#1490),#1886,.T.);
#12388=ADVANCED_FACE('',(#2663,#1491),#1887,.F.);
#12389=ADVANCED_FACE('',(#2664),#11614,.T.);
#12390=ADVANCED_FACE('',(#2665),#1888,.T.);
#12391=ADVANCED_FACE('',(#2666),#1889,.F.);
#12392=CLOSED_SHELL('',(#11615,#11616,#11617,#11618,#11619,#11620,#11621,
#11622,#11623,#11624,#11625,#11626,#11627,#11628,#11629,#11630,#11631,#11632));
#12393=CLOSED_SHELL('',(#11633,#11634,#11635,#11636,#11637,#11638));
#12394=CLOSED_SHELL('',(#11639,#11640,#11641,#11642,#11643,#11644));
#12395=CLOSED_SHELL('',(#11645,#11646,#11647,#11648,#11649,#11650,#11651,
#11652,#11653,#11654,#11655,#11656,#11657,#11658,#11659,#11660,#11661,#11662));
#12396=CLOSED_SHELL('',(#11663,#11664,#11665,#11666,#11667,#11668,#11669,
#11670,#11671,#11672,#11673,#11674,#11675,#11676,#11677,#11678,#11679,#11680));
#12397=CLOSED_SHELL('',(#11681,#11682,#11683,#11684,#11685,#11686,#11687,
#11688,#11689,#11690,#11691,#11692));
#12398=CLOSED_SHELL('',(#11693,#11694,#11695,#11696));
#12399=CLOSED_SHELL('',(#11697,#11698,#11699,#11700));
#12400=CLOSED_SHELL('',(#11701,#11702,#11703,#11704));
#12401=CLOSED_SHELL('',(#11705,#11706,#11707,#11708,#11709,#11710,#11711,
#11712,#11713,#11714,#11715,#11716));
#12402=CLOSED_SHELL('',(#11717,#11718,#11719,#11720));
#12403=CLOSED_SHELL('',(#11721,#11722,#11723,#11724));
#12404=CLOSED_SHELL('',(#11725,#11726,#11727,#11728));
#12405=CLOSED_SHELL('',(#11729,#11730,#11731,#11732,#11733,#11734,#11735,
#11736,#11737,#11738,#11739,#11740,#11741,#11742,#11743,#11744,#11745,#11746));
#12406=CLOSED_SHELL('',(#11747,#11748,#11749,#11750,#11751,#11752,#11753,
#11754,#11755));
#12407=CLOSED_SHELL('',(#11756,#11757,#11758,#11759,#11760));
#12408=CLOSED_SHELL('',(#11761,#11762,#11763,#11764,#11765));
#12409=CLOSED_SHELL('',(#11766,#11767,#11768,#11769,#11770,#11771,#11772,
#11773,#11774));
#12410=CLOSED_SHELL('',(#11775,#11776,#11777,#11778,#11779));
#12411=CLOSED_SHELL('',(#11780,#11781,#11782,#11783,#11784));
#12412=CLOSED_SHELL('',(#11785,#11786,#11787,#11788,#11789,#11790,#11791,
#11792,#11793,#11794,#11795,#11796,#11797,#11798,#11799,#11800,#11801,#11802));
#12413=CLOSED_SHELL('',(#11803,#11804,#11805,#11806,#11807,#11808,#11809,
#11810,#11811));
#12414=CLOSED_SHELL('',(#11812,#11813,#11814,#11815,#11816));
#12415=CLOSED_SHELL('',(#11817,#11818,#11819,#11820,#11821));
#12416=CLOSED_SHELL('',(#11822,#11823,#11824,#11825,#11826,#11827,#11828,
#11829,#11830));
#12417=CLOSED_SHELL('',(#11831,#11832,#11833,#11834,#11835));
#12418=CLOSED_SHELL('',(#11836,#11837,#11838,#11839,#11840));
#12419=CLOSED_SHELL('',(#11841,#11842,#11843));
#12420=CLOSED_SHELL('',(#11844,#11845,#11846));
#12421=CLOSED_SHELL('',(#11847,#11848,#11849,#11850,#11851,#11852,#11853,
#11854,#11855));
#12422=CLOSED_SHELL('',(#11856,#11857,#11858,#11859,#11860,#11861,#11862,
#11863));
#12423=CLOSED_SHELL('',(#11864,#11865,#11866,#11867,#11868,#11869,#11870,
#11871,#11872,#11873,#11874,#11875,#11876,#11877,#11878,#11879));
#12424=CLOSED_SHELL('',(#11880,#11881,#11882,#11883,#11884,#11885,#11886,
#11887));
#12425=CLOSED_SHELL('',(#11888,#11889,#11890,#11891,#11892));
#12426=CLOSED_SHELL('',(#11893,#11894,#11895,#11896,#11897));
#12427=CLOSED_SHELL('',(#11898,#11899,#11900,#11901,#11902));
#12428=CLOSED_SHELL('',(#11903,#11904,#11905,#11906,#11907));
#12429=CLOSED_SHELL('',(#11908,#11909,#11910,#11911,#11912,#11913,#11914,
#11915));
#12430=CLOSED_SHELL('',(#11916,#11917,#11918,#11919,#11920));
#12431=CLOSED_SHELL('',(#11921,#11922,#11923,#11924,#11925));
#12432=CLOSED_SHELL('',(#11926,#11927,#11928,#11929,#11930));
#12433=CLOSED_SHELL('',(#11931,#11932,#11933,#11934,#11935));
#12434=CLOSED_SHELL('',(#11936,#11937,#11938,#11939,#11940,#11941,#11942,
#11943));
#12435=CLOSED_SHELL('',(#11944,#11945,#11946,#11947,#11948));
#12436=CLOSED_SHELL('',(#11949,#11950,#11951,#11952,#11953));
#12437=CLOSED_SHELL('',(#11954,#11955,#11956,#11957,#11958));
#12438=CLOSED_SHELL('',(#11959,#11960,#11961,#11962,#11963));
#12439=CLOSED_SHELL('',(#11964,#11965,#11966,#11967,#11968,#11969,#11970,
#11971));
#12440=CLOSED_SHELL('',(#11972,#11973,#11974,#11975,#11976));
#12441=CLOSED_SHELL('',(#11977,#11978,#11979,#11980,#11981));
#12442=CLOSED_SHELL('',(#11982,#11983,#11984,#11985,#11986));
#12443=CLOSED_SHELL('',(#11987,#11988,#11989,#11990,#11991));
#12444=CLOSED_SHELL('',(#11992,#11993,#11994,#11995,#11996,#11997,#11998,
#11999,#12000,#12001,#12002,#12003,#12004,#12005,#12006,#12007));
#12445=CLOSED_SHELL('',(#12008,#12009,#12010,#12011,#12012,#12013,#12014,
#12015));
#12446=CLOSED_SHELL('',(#12016,#12017,#12018,#12019,#12020));
#12447=CLOSED_SHELL('',(#12021,#12022,#12023,#12024,#12025));
#12448=CLOSED_SHELL('',(#12026,#12027,#12028,#12029,#12030));
#12449=CLOSED_SHELL('',(#12031,#12032,#12033,#12034,#12035));
#12450=CLOSED_SHELL('',(#12036,#12037,#12038,#12039,#12040,#12041,#12042,
#12043));
#12451=CLOSED_SHELL('',(#12044,#12045,#12046,#12047,#12048));
#12452=CLOSED_SHELL('',(#12049,#12050,#12051,#12052,#12053));
#12453=CLOSED_SHELL('',(#12054,#12055,#12056,#12057,#12058));
#12454=CLOSED_SHELL('',(#12059,#12060,#12061,#12062,#12063));
#12455=CLOSED_SHELL('',(#12064,#12065,#12066,#12067,#12068,#12069,#12070,
#12071));
#12456=CLOSED_SHELL('',(#12072,#12073,#12074,#12075,#12076));
#12457=CLOSED_SHELL('',(#12077,#12078,#12079,#12080,#12081));
#12458=CLOSED_SHELL('',(#12082,#12083,#12084,#12085,#12086));
#12459=CLOSED_SHELL('',(#12087,#12088,#12089,#12090,#12091));
#12460=CLOSED_SHELL('',(#12092,#12093,#12094,#12095,#12096,#12097,#12098,
#12099));
#12461=CLOSED_SHELL('',(#12100,#12101,#12102,#12103,#12104));
#12462=CLOSED_SHELL('',(#12105,#12106,#12107,#12108,#12109));
#12463=CLOSED_SHELL('',(#12110,#12111,#12112,#12113,#12114));
#12464=CLOSED_SHELL('',(#12115,#12116,#12117,#12118,#12119));
#12465=CLOSED_SHELL('',(#12120,#12121,#12122,#12123,#12124,#12125,#12126,
#12127));
#12466=CLOSED_SHELL('',(#12128,#12129,#12130,#12131,#12132,#12133,#12134,
#12135));
#12467=CLOSED_SHELL('',(#12136));
#12468=CLOSED_SHELL('',(#12137));
#12469=CLOSED_SHELL('',(#12138));
#12470=CLOSED_SHELL('',(#12139));
#12471=CLOSED_SHELL('',(#12140));
#12472=CLOSED_SHELL('',(#12141));
#12473=CLOSED_SHELL('',(#12142));
#12474=CLOSED_SHELL('',(#12143,#12144,#12145,#12146,#12147,#12148,#12149,
#12150,#12151,#12152,#12153,#12154,#12155,#12156,#12157,#12158,#12159));
#12475=CLOSED_SHELL('',(#12160,#12161,#12162,#12163));
#12476=CLOSED_SHELL('',(#12164,#12165,#12166,#12167));
#12477=CLOSED_SHELL('',(#12168,#12169,#12170,#12171,#12172,#12173,#12174,
#12175,#12176,#12177,#12178,#12179,#12180,#12181,#12182,#12183,#12184,#12185,
#12186,#12187,#12188));
#12478=CLOSED_SHELL('',(#12189,#12190,#12191,#12192,#12193,#12194));
#12479=CLOSED_SHELL('',(#12195,#12196,#12197,#12198,#12199,#12200));
#12480=CLOSED_SHELL('',(#12201,#12202,#12203,#12204,#12205,#12206));
#12481=CLOSED_SHELL('',(#12207,#12208,#12209,#12210,#12211,#12212,#12213,
#12214,#12215,#12216,#12217,#12218));
#12482=CLOSED_SHELL('',(#12219,#12220,#12221,#12222));
#12483=CLOSED_SHELL('',(#12223,#12224,#12225,#12226));
#12484=CLOSED_SHELL('',(#12227,#12228,#12229,#12230));
#12485=CLOSED_SHELL('',(#12231,#12232,#12233,#12234));
#12486=CLOSED_SHELL('',(#12235,#12236,#12237,#12238,#12239,#12240,#12241,
#12242,#12243,#12244,#12245,#12246));
#12487=CLOSED_SHELL('',(#12247,#12248,#12249,#12250));
#12488=CLOSED_SHELL('',(#12251,#12252,#12253,#12254));
#12489=CLOSED_SHELL('',(#12255,#12256,#12257,#12258));
#12490=CLOSED_SHELL('',(#12259,#12260,#12261,#12262,#12263,#12264,#12265,
#12266,#12267));
#12491=CLOSED_SHELL('',(#12268,#12269,#12270,#12271,#12272,#12273,#12274,
#12275));
#12492=CLOSED_SHELL('',(#12276,#12277,#12278,#12279,#12280,#12281,#12282,
#12283,#12284));
#12493=CLOSED_SHELL('',(#12285,#12286,#12287,#12288,#12289,#12290,#12291,
#12292,#12293));
#12494=CLOSED_SHELL('',(#12294,#12295,#12296,#12297,#12298,#12299,#12300,
#12301,#12302));
#12495=CLOSED_SHELL('',(#12303,#12304,#12305,#12306,#12307,#12308,#12309));
#12496=CLOSED_SHELL('',(#12310,#12311,#12312,#12313,#12314,#12315,#12316));
#12497=CLOSED_SHELL('',(#12317,#12318,#12319,#12320));
#12498=CLOSED_SHELL('',(#12321,#12322,#12323,#12324));
#12499=CLOSED_SHELL('',(#12325,#12326,#12327,#12328,#12329,#12330,#12331,
#12332,#12333,#12334,#12335,#12336,#12337,#12338,#12339,#12340,#12341));
#12500=CLOSED_SHELL('',(#12342,#12343,#12344,#12345,#12346,#12347,#12348,
#12349));
#12501=CLOSED_SHELL('',(#12350,#12351,#12352,#12353,#12354,#12355,#12356,
#12357));
#12502=CLOSED_SHELL('',(#12358,#12359,#12360,#12361,#12362,#12363,#12364,
#12365));
#12503=CLOSED_SHELL('',(#12366,#12367,#12368,#12369,#12370,#12371,#12372,
#12373));
#12504=CLOSED_SHELL('',(#12374,#12375,#12376));
#12505=CLOSED_SHELL('',(#12377,#12378,#12379,#12380));
#12506=CLOSED_SHELL('',(#12381,#12382,#12383,#12384));
#12507=CLOSED_SHELL('',(#12385,#12386,#12387,#12388));
#12508=CLOSED_SHELL('',(#12389,#12390,#12391));
#12509=DERIVED_UNIT_ELEMENT(#12721,1.);
#12510=DERIVED_UNIT_ELEMENT(#23730,-3.);
#12511=DERIVED_UNIT_ELEMENT(#12721,1.);
#12512=DERIVED_UNIT_ELEMENT(#23730,-3.);
#12513=DERIVED_UNIT_ELEMENT(#12721,1.);
#12514=DERIVED_UNIT_ELEMENT(#23730,-3.);
#12515=DERIVED_UNIT_ELEMENT(#12721,1.);
#12516=DERIVED_UNIT_ELEMENT(#23730,-3.);
#12517=DERIVED_UNIT_ELEMENT(#12721,1.);
#12518=DERIVED_UNIT_ELEMENT(#23730,-3.);
#12519=DERIVED_UNIT_ELEMENT(#12721,1.);
#12520=DERIVED_UNIT_ELEMENT(#23730,-3.);
#12521=DERIVED_UNIT_ELEMENT(#12721,1.);
#12522=DERIVED_UNIT_ELEMENT(#23730,-3.);
#12523=DERIVED_UNIT_ELEMENT(#12721,1.);
#12524=DERIVED_UNIT_ELEMENT(#23730,-3.);
#12525=DERIVED_UNIT_ELEMENT(#12721,1.);
#12526=DERIVED_UNIT_ELEMENT(#23730,-3.);
#12527=DERIVED_UNIT_ELEMENT(#12721,1.);
#12528=DERIVED_UNIT_ELEMENT(#23730,-3.);
#12529=DERIVED_UNIT_ELEMENT(#12721,1.);
#12530=DERIVED_UNIT_ELEMENT(#23730,-3.);
#12531=DERIVED_UNIT_ELEMENT(#12721,1.);
#12532=DERIVED_UNIT_ELEMENT(#23730,-3.);
#12533=DERIVED_UNIT_ELEMENT(#12721,1.);
#12534=DERIVED_UNIT_ELEMENT(#23730,-3.);
#12535=DERIVED_UNIT_ELEMENT(#12721,1.);
#12536=DERIVED_UNIT_ELEMENT(#23730,-3.);
#12537=DERIVED_UNIT_ELEMENT(#12721,1.);
#12538=DERIVED_UNIT_ELEMENT(#23730,-3.);
#12539=DERIVED_UNIT_ELEMENT(#12721,1.);
#12540=DERIVED_UNIT_ELEMENT(#23730,-3.);
#12541=DERIVED_UNIT_ELEMENT(#12721,1.);
#12542=DERIVED_UNIT_ELEMENT(#23730,-3.);
#12543=DERIVED_UNIT_ELEMENT(#12721,1.);
#12544=DERIVED_UNIT_ELEMENT(#23730,-3.);
#12545=DERIVED_UNIT_ELEMENT(#12721,1.);
#12546=DERIVED_UNIT_ELEMENT(#23730,-3.);
#12547=DERIVED_UNIT_ELEMENT(#12721,1.);
#12548=DERIVED_UNIT_ELEMENT(#23730,-3.);
#12549=DERIVED_UNIT_ELEMENT(#12721,1.);
#12550=DERIVED_UNIT_ELEMENT(#23730,-3.);
#12551=DERIVED_UNIT_ELEMENT(#12721,1.);
#12552=DERIVED_UNIT_ELEMENT(#23730,-3.);
#12553=DERIVED_UNIT_ELEMENT(#12721,1.);
#12554=DERIVED_UNIT_ELEMENT(#23730,-3.);
#12555=DERIVED_UNIT_ELEMENT(#12721,1.);
#12556=DERIVED_UNIT_ELEMENT(#23730,-3.);
#12557=DERIVED_UNIT_ELEMENT(#12721,1.);
#12558=DERIVED_UNIT_ELEMENT(#23730,-3.);
#12559=DERIVED_UNIT_ELEMENT(#12721,1.);
#12560=DERIVED_UNIT_ELEMENT(#23730,-3.);
#12561=DERIVED_UNIT_ELEMENT(#12721,1.);
#12562=DERIVED_UNIT_ELEMENT(#23730,-3.);
#12563=DERIVED_UNIT_ELEMENT(#12721,1.);
#12564=DERIVED_UNIT_ELEMENT(#23730,-3.);
#12565=DERIVED_UNIT_ELEMENT(#12721,1.);
#12566=DERIVED_UNIT_ELEMENT(#23730,-3.);
#12567=DERIVED_UNIT_ELEMENT(#12721,1.);
#12568=DERIVED_UNIT_ELEMENT(#23730,-3.);
#12569=DERIVED_UNIT_ELEMENT(#12721,1.);
#12570=DERIVED_UNIT_ELEMENT(#23730,-3.);
#12571=DERIVED_UNIT_ELEMENT(#12721,1.);
#12572=DERIVED_UNIT_ELEMENT(#23730,-3.);
#12573=DERIVED_UNIT_ELEMENT(#12721,1.);
#12574=DERIVED_UNIT_ELEMENT(#23730,-3.);
#12575=DERIVED_UNIT_ELEMENT(#12721,1.);
#12576=DERIVED_UNIT_ELEMENT(#23730,-3.);
#12577=DERIVED_UNIT_ELEMENT(#12721,1.);
#12578=DERIVED_UNIT_ELEMENT(#23730,-3.);
#12579=DERIVED_UNIT_ELEMENT(#12721,1.);
#12580=DERIVED_UNIT_ELEMENT(#23730,-3.);
#12581=DERIVED_UNIT_ELEMENT(#12721,1.);
#12582=DERIVED_UNIT_ELEMENT(#23730,-3.);
#12583=DERIVED_UNIT_ELEMENT(#12721,1.);
#12584=DERIVED_UNIT_ELEMENT(#23730,-3.);
#12585=DERIVED_UNIT_ELEMENT(#12721,1.);
#12586=DERIVED_UNIT_ELEMENT(#23730,-3.);
#12587=DERIVED_UNIT_ELEMENT(#12721,1.);
#12588=DERIVED_UNIT_ELEMENT(#23730,-3.);
#12589=DERIVED_UNIT_ELEMENT(#12721,1.);
#12590=DERIVED_UNIT_ELEMENT(#23730,-3.);
#12591=DERIVED_UNIT_ELEMENT(#12721,1.);
#12592=DERIVED_UNIT_ELEMENT(#23730,-3.);
#12593=DERIVED_UNIT_ELEMENT(#12721,1.);
#12594=DERIVED_UNIT_ELEMENT(#23730,-3.);
#12595=DERIVED_UNIT_ELEMENT(#12721,1.);
#12596=DERIVED_UNIT_ELEMENT(#23730,-3.);
#12597=DERIVED_UNIT_ELEMENT(#12721,1.);
#12598=DERIVED_UNIT_ELEMENT(#23730,-3.);
#12599=DERIVED_UNIT_ELEMENT(#12721,1.);
#12600=DERIVED_UNIT_ELEMENT(#23730,-3.);
#12601=DERIVED_UNIT_ELEMENT(#12721,1.);
#12602=DERIVED_UNIT_ELEMENT(#23730,-3.);
#12603=DERIVED_UNIT_ELEMENT(#12721,1.);
#12604=DERIVED_UNIT_ELEMENT(#23730,-3.);
#12605=DERIVED_UNIT_ELEMENT(#12721,1.);
#12606=DERIVED_UNIT_ELEMENT(#23730,-3.);
#12607=DERIVED_UNIT_ELEMENT(#12721,1.);
#12608=DERIVED_UNIT_ELEMENT(#23730,-3.);
#12609=DERIVED_UNIT_ELEMENT(#12721,1.);
#12610=DERIVED_UNIT_ELEMENT(#23730,-3.);
#12611=DERIVED_UNIT_ELEMENT(#12721,1.);
#12612=DERIVED_UNIT_ELEMENT(#23730,-3.);
#12613=DERIVED_UNIT_ELEMENT(#12721,1.);
#12614=DERIVED_UNIT_ELEMENT(#23730,-3.);
#12615=DERIVED_UNIT_ELEMENT(#12721,1.);
#12616=DERIVED_UNIT_ELEMENT(#23730,-3.);
#12617=DERIVED_UNIT_ELEMENT(#12721,1.);
#12618=DERIVED_UNIT_ELEMENT(#23730,-3.);
#12619=DERIVED_UNIT_ELEMENT(#12721,1.);
#12620=DERIVED_UNIT_ELEMENT(#23730,-3.);
#12621=DERIVED_UNIT_ELEMENT(#12721,1.);
#12622=DERIVED_UNIT_ELEMENT(#23730,-3.);
#12623=DERIVED_UNIT_ELEMENT(#12721,1.);
#12624=DERIVED_UNIT_ELEMENT(#23730,-3.);
#12625=DERIVED_UNIT_ELEMENT(#12721,1.);
#12626=DERIVED_UNIT_ELEMENT(#23730,-3.);
#12627=DERIVED_UNIT_ELEMENT(#12721,1.);
#12628=DERIVED_UNIT_ELEMENT(#23730,-3.);
#12629=DERIVED_UNIT_ELEMENT(#12721,1.);
#12630=DERIVED_UNIT_ELEMENT(#23730,-3.);
#12631=DERIVED_UNIT_ELEMENT(#12721,1.);
#12632=DERIVED_UNIT_ELEMENT(#23730,-3.);
#12633=DERIVED_UNIT_ELEMENT(#12721,1.);
#12634=DERIVED_UNIT_ELEMENT(#23730,-3.);
#12635=DERIVED_UNIT_ELEMENT(#12721,1.);
#12636=DERIVED_UNIT_ELEMENT(#23730,-3.);
#12637=DERIVED_UNIT_ELEMENT(#12721,1.);
#12638=DERIVED_UNIT_ELEMENT(#23730,-3.);
#12639=DERIVED_UNIT_ELEMENT(#12721,1.);
#12640=DERIVED_UNIT_ELEMENT(#23730,-3.);
#12641=DERIVED_UNIT_ELEMENT(#12721,1.);
#12642=DERIVED_UNIT_ELEMENT(#23730,-3.);
#12643=DERIVED_UNIT_ELEMENT(#12721,1.);
#12644=DERIVED_UNIT_ELEMENT(#23730,-3.);
#12645=DERIVED_UNIT_ELEMENT(#12721,1.);
#12646=DERIVED_UNIT_ELEMENT(#23730,-3.);
#12647=DERIVED_UNIT_ELEMENT(#12721,1.);
#12648=DERIVED_UNIT_ELEMENT(#23730,-3.);
#12649=DERIVED_UNIT_ELEMENT(#12721,1.);
#12650=DERIVED_UNIT_ELEMENT(#23730,-3.);
#12651=DERIVED_UNIT_ELEMENT(#12721,1.);
#12652=DERIVED_UNIT_ELEMENT(#23730,-3.);
#12653=DERIVED_UNIT_ELEMENT(#12721,1.);
#12654=DERIVED_UNIT_ELEMENT(#23730,-3.);
#12655=DERIVED_UNIT_ELEMENT(#12721,1.);
#12656=DERIVED_UNIT_ELEMENT(#23730,-3.);
#12657=DERIVED_UNIT_ELEMENT(#12721,1.);
#12658=DERIVED_UNIT_ELEMENT(#23730,-3.);
#12659=DERIVED_UNIT_ELEMENT(#12721,1.);
#12660=DERIVED_UNIT_ELEMENT(#23730,-3.);
#12661=DERIVED_UNIT_ELEMENT(#12721,1.);
#12662=DERIVED_UNIT_ELEMENT(#23730,-3.);
#12663=DERIVED_UNIT_ELEMENT(#12721,1.);
#12664=DERIVED_UNIT_ELEMENT(#23730,-3.);
#12665=DERIVED_UNIT_ELEMENT(#12721,1.);
#12666=DERIVED_UNIT_ELEMENT(#23730,-3.);
#12667=DERIVED_UNIT_ELEMENT(#12721,1.);
#12668=DERIVED_UNIT_ELEMENT(#23730,-3.);
#12669=DERIVED_UNIT_ELEMENT(#12721,1.);
#12670=DERIVED_UNIT_ELEMENT(#23730,-3.);
#12671=DERIVED_UNIT_ELEMENT(#12721,1.);
#12672=DERIVED_UNIT_ELEMENT(#23730,-3.);
#12673=DERIVED_UNIT_ELEMENT(#12721,1.);
#12674=DERIVED_UNIT_ELEMENT(#23730,-3.);
#12675=DERIVED_UNIT_ELEMENT(#12721,1.);
#12676=DERIVED_UNIT_ELEMENT(#23730,-3.);
#12677=DERIVED_UNIT_ELEMENT(#12721,1.);
#12678=DERIVED_UNIT_ELEMENT(#23730,-3.);
#12679=DERIVED_UNIT_ELEMENT(#12721,1.);
#12680=DERIVED_UNIT_ELEMENT(#23730,-3.);
#12681=DERIVED_UNIT_ELEMENT(#12721,1.);
#12682=DERIVED_UNIT_ELEMENT(#23730,-3.);
#12683=DERIVED_UNIT_ELEMENT(#12721,1.);
#12684=DERIVED_UNIT_ELEMENT(#23730,-3.);
#12685=DERIVED_UNIT_ELEMENT(#12721,1.);
#12686=DERIVED_UNIT_ELEMENT(#23730,-3.);
#12687=DERIVED_UNIT_ELEMENT(#12721,1.);
#12688=DERIVED_UNIT_ELEMENT(#23730,-3.);
#12689=DERIVED_UNIT_ELEMENT(#12721,1.);
#12690=DERIVED_UNIT_ELEMENT(#23730,-3.);
#12691=DERIVED_UNIT_ELEMENT(#12721,1.);
#12692=DERIVED_UNIT_ELEMENT(#23730,-3.);
#12693=DERIVED_UNIT_ELEMENT(#12721,1.);
#12694=DERIVED_UNIT_ELEMENT(#23730,-3.);
#12695=DERIVED_UNIT_ELEMENT(#12721,1.);
#12696=DERIVED_UNIT_ELEMENT(#23730,-3.);
#12697=DERIVED_UNIT_ELEMENT(#12721,1.);
#12698=DERIVED_UNIT_ELEMENT(#23730,-3.);
#12699=DERIVED_UNIT_ELEMENT(#12721,1.);
#12700=DERIVED_UNIT_ELEMENT(#23730,-3.);
#12701=DERIVED_UNIT_ELEMENT(#12721,1.);
#12702=DERIVED_UNIT_ELEMENT(#23730,-3.);
#12703=DERIVED_UNIT_ELEMENT(#12721,1.);
#12704=DERIVED_UNIT_ELEMENT(#23730,-3.);
#12705=DERIVED_UNIT_ELEMENT(#12721,1.);
#12706=DERIVED_UNIT_ELEMENT(#23730,-3.);
#12707=DERIVED_UNIT_ELEMENT(#12721,1.);
#12708=DERIVED_UNIT_ELEMENT(#23730,-3.);
#12709=DERIVED_UNIT_ELEMENT(#12721,1.);
#12710=DERIVED_UNIT_ELEMENT(#23730,-3.);
#12711=DERIVED_UNIT_ELEMENT(#12721,1.);
#12712=DERIVED_UNIT_ELEMENT(#23730,-3.);
#12713=DERIVED_UNIT_ELEMENT(#12721,1.);
#12714=DERIVED_UNIT_ELEMENT(#23730,-3.);
#12715=DERIVED_UNIT_ELEMENT(#12721,1.);
#12716=DERIVED_UNIT_ELEMENT(#23730,-3.);
#12717=DERIVED_UNIT_ELEMENT(#12721,1.);
#12718=DERIVED_UNIT_ELEMENT(#23730,-3.);
#12719=DERIVED_UNIT_ELEMENT(#12721,1.);
#12720=DERIVED_UNIT_ELEMENT(#23730,-3.);
#12721=(
MASS_UNIT()
NAMED_UNIT(*)
SI_UNIT(.KILO.,.GRAM.)
);
#12722=DERIVED_UNIT((#12509,#12510));
#12723=DERIVED_UNIT((#12511,#12512));
#12724=DERIVED_UNIT((#12513,#12514));
#12725=DERIVED_UNIT((#12515,#12516));
#12726=DERIVED_UNIT((#12517,#12518));
#12727=DERIVED_UNIT((#12519,#12520));
#12728=DERIVED_UNIT((#12521,#12522));
#12729=DERIVED_UNIT((#12523,#12524));
#12730=DERIVED_UNIT((#12525,#12526));
#12731=DERIVED_UNIT((#12527,#12528));
#12732=DERIVED_UNIT((#12529,#12530));
#12733=DERIVED_UNIT((#12531,#12532));
#12734=DERIVED_UNIT((#12533,#12534));
#12735=DERIVED_UNIT((#12535,#12536));
#12736=DERIVED_UNIT((#12537,#12538));
#12737=DERIVED_UNIT((#12539,#12540));
#12738=DERIVED_UNIT((#12541,#12542));
#12739=DERIVED_UNIT((#12543,#12544));
#12740=DERIVED_UNIT((#12545,#12546));
#12741=DERIVED_UNIT((#12547,#12548));
#12742=DERIVED_UNIT((#12549,#12550));
#12743=DERIVED_UNIT((#12551,#12552));
#12744=DERIVED_UNIT((#12553,#12554));
#12745=DERIVED_UNIT((#12555,#12556));
#12746=DERIVED_UNIT((#12557,#12558));
#12747=DERIVED_UNIT((#12559,#12560));
#12748=DERIVED_UNIT((#12561,#12562));
#12749=DERIVED_UNIT((#12563,#12564));
#12750=DERIVED_UNIT((#12565,#12566));
#12751=DERIVED_UNIT((#12567,#12568));
#12752=DERIVED_UNIT((#12569,#12570));
#12753=DERIVED_UNIT((#12571,#12572));
#12754=DERIVED_UNIT((#12573,#12574));
#12755=DERIVED_UNIT((#12575,#12576));
#12756=DERIVED_UNIT((#12577,#12578));
#12757=DERIVED_UNIT((#12579,#12580));
#12758=DERIVED_UNIT((#12581,#12582));
#12759=DERIVED_UNIT((#12583,#12584));
#12760=DERIVED_UNIT((#12585,#12586));
#12761=DERIVED_UNIT((#12587,#12588));
#12762=DERIVED_UNIT((#12589,#12590));
#12763=DERIVED_UNIT((#12591,#12592));
#12764=DERIVED_UNIT((#12593,#12594));
#12765=DERIVED_UNIT((#12595,#12596));
#12766=DERIVED_UNIT((#12597,#12598));
#12767=DERIVED_UNIT((#12599,#12600));
#12768=DERIVED_UNIT((#12601,#12602));
#12769=DERIVED_UNIT((#12603,#12604));
#12770=DERIVED_UNIT((#12605,#12606));
#12771=DERIVED_UNIT((#12607,#12608));
#12772=DERIVED_UNIT((#12609,#12610));
#12773=DERIVED_UNIT((#12611,#12612));
#12774=DERIVED_UNIT((#12613,#12614));
#12775=DERIVED_UNIT((#12615,#12616));
#12776=DERIVED_UNIT((#12617,#12618));
#12777=DERIVED_UNIT((#12619,#12620));
#12778=DERIVED_UNIT((#12621,#12622));
#12779=DERIVED_UNIT((#12623,#12624));
#12780=DERIVED_UNIT((#12625,#12626));
#12781=DERIVED_UNIT((#12627,#12628));
#12782=DERIVED_UNIT((#12629,#12630));
#12783=DERIVED_UNIT((#12631,#12632));
#12784=DERIVED_UNIT((#12633,#12634));
#12785=DERIVED_UNIT((#12635,#12636));
#12786=DERIVED_UNIT((#12637,#12638));
#12787=DERIVED_UNIT((#12639,#12640));
#12788=DERIVED_UNIT((#12641,#12642));
#12789=DERIVED_UNIT((#12643,#12644));
#12790=DERIVED_UNIT((#12645,#12646));
#12791=DERIVED_UNIT((#12647,#12648));
#12792=DERIVED_UNIT((#12649,#12650));
#12793=DERIVED_UNIT((#12651,#12652));
#12794=DERIVED_UNIT((#12653,#12654));
#12795=DERIVED_UNIT((#12655,#12656));
#12796=DERIVED_UNIT((#12657,#12658));
#12797=DERIVED_UNIT((#12659,#12660));
#12798=DERIVED_UNIT((#12661,#12662));
#12799=DERIVED_UNIT((#12663,#12664));
#12800=DERIVED_UNIT((#12665,#12666));
#12801=DERIVED_UNIT((#12667,#12668));
#12802=DERIVED_UNIT((#12669,#12670));
#12803=DERIVED_UNIT((#12671,#12672));
#12804=DERIVED_UNIT((#12673,#12674));
#12805=DERIVED_UNIT((#12675,#12676));
#12806=DERIVED_UNIT((#12677,#12678));
#12807=DERIVED_UNIT((#12679,#12680));
#12808=DERIVED_UNIT((#12681,#12682));
#12809=DERIVED_UNIT((#12683,#12684));
#12810=DERIVED_UNIT((#12685,#12686));
#12811=DERIVED_UNIT((#12687,#12688));
#12812=DERIVED_UNIT((#12689,#12690));
#12813=DERIVED_UNIT((#12691,#12692));
#12814=DERIVED_UNIT((#12693,#12694));
#12815=DERIVED_UNIT((#12695,#12696));
#12816=DERIVED_UNIT((#12697,#12698));
#12817=DERIVED_UNIT((#12699,#12700));
#12818=DERIVED_UNIT((#12701,#12702));
#12819=DERIVED_UNIT((#12703,#12704));
#12820=DERIVED_UNIT((#12705,#12706));
#12821=DERIVED_UNIT((#12707,#12708));
#12822=DERIVED_UNIT((#12709,#12710));
#12823=DERIVED_UNIT((#12711,#12712));
#12824=DERIVED_UNIT((#12713,#12714));
#12825=DERIVED_UNIT((#12715,#12716));
#12826=DERIVED_UNIT((#12717,#12718));
#12827=DERIVED_UNIT((#12719,#12720));
#12828=MEASURE_REPRESENTATION_ITEM('density measure',
POSITIVE_RATIO_MEASURE(7850.),#12722);
#12829=MEASURE_REPRESENTATION_ITEM('density measure',
POSITIVE_RATIO_MEASURE(7850.),#12723);
#12830=MEASURE_REPRESENTATION_ITEM('density measure',
POSITIVE_RATIO_MEASURE(7850.),#12724);
#12831=MEASURE_REPRESENTATION_ITEM('density measure',
POSITIVE_RATIO_MEASURE(7850.),#12725);
#12832=MEASURE_REPRESENTATION_ITEM('density measure',
POSITIVE_RATIO_MEASURE(7850.),#12726);
#12833=MEASURE_REPRESENTATION_ITEM('density measure',
POSITIVE_RATIO_MEASURE(7850.),#12727);
#12834=MEASURE_REPRESENTATION_ITEM('density measure',
POSITIVE_RATIO_MEASURE(7850.),#12728);
#12835=MEASURE_REPRESENTATION_ITEM('density measure',
POSITIVE_RATIO_MEASURE(7850.),#12729);
#12836=MEASURE_REPRESENTATION_ITEM('density measure',
POSITIVE_RATIO_MEASURE(7850.),#12730);
#12837=MEASURE_REPRESENTATION_ITEM('density measure',
POSITIVE_RATIO_MEASURE(7850.),#12731);
#12838=MEASURE_REPRESENTATION_ITEM('density measure',
POSITIVE_RATIO_MEASURE(7850.),#12732);
#12839=MEASURE_REPRESENTATION_ITEM('density measure',
POSITIVE_RATIO_MEASURE(7850.),#12733);
#12840=MEASURE_REPRESENTATION_ITEM('density measure',
POSITIVE_RATIO_MEASURE(7850.),#12734);
#12841=MEASURE_REPRESENTATION_ITEM('density measure',
POSITIVE_RATIO_MEASURE(7850.),#12735);
#12842=MEASURE_REPRESENTATION_ITEM('density measure',
POSITIVE_RATIO_MEASURE(7850.),#12736);
#12843=MEASURE_REPRESENTATION_ITEM('density measure',
POSITIVE_RATIO_MEASURE(7850.),#12737);
#12844=MEASURE_REPRESENTATION_ITEM('density measure',
POSITIVE_RATIO_MEASURE(7850.),#12738);
#12845=MEASURE_REPRESENTATION_ITEM('density measure',
POSITIVE_RATIO_MEASURE(7850.),#12739);
#12846=MEASURE_REPRESENTATION_ITEM('density measure',
POSITIVE_RATIO_MEASURE(7850.),#12740);
#12847=MEASURE_REPRESENTATION_ITEM('density measure',
POSITIVE_RATIO_MEASURE(7850.),#12741);
#12848=MEASURE_REPRESENTATION_ITEM('density measure',
POSITIVE_RATIO_MEASURE(7850.),#12742);
#12849=MEASURE_REPRESENTATION_ITEM('density measure',
POSITIVE_RATIO_MEASURE(7850.),#12743);
#12850=MEASURE_REPRESENTATION_ITEM('density measure',
POSITIVE_RATIO_MEASURE(7850.),#12744);
#12851=MEASURE_REPRESENTATION_ITEM('density measure',
POSITIVE_RATIO_MEASURE(7850.),#12745);
#12852=MEASURE_REPRESENTATION_ITEM('density measure',
POSITIVE_RATIO_MEASURE(7850.),#12746);
#12853=MEASURE_REPRESENTATION_ITEM('density measure',
POSITIVE_RATIO_MEASURE(7850.),#12747);
#12854=MEASURE_REPRESENTATION_ITEM('density measure',
POSITIVE_RATIO_MEASURE(7850.),#12748);
#12855=MEASURE_REPRESENTATION_ITEM('density measure',
POSITIVE_RATIO_MEASURE(7850.),#12749);
#12856=MEASURE_REPRESENTATION_ITEM('density measure',
POSITIVE_RATIO_MEASURE(7850.),#12750);
#12857=MEASURE_REPRESENTATION_ITEM('density measure',
POSITIVE_RATIO_MEASURE(7850.),#12751);
#12858=MEASURE_REPRESENTATION_ITEM('density measure',
POSITIVE_RATIO_MEASURE(7850.),#12752);
#12859=MEASURE_REPRESENTATION_ITEM('density measure',
POSITIVE_RATIO_MEASURE(7850.),#12753);
#12860=MEASURE_REPRESENTATION_ITEM('density measure',
POSITIVE_RATIO_MEASURE(7850.),#12754);
#12861=MEASURE_REPRESENTATION_ITEM('density measure',
POSITIVE_RATIO_MEASURE(7850.),#12755);
#12862=MEASURE_REPRESENTATION_ITEM('density measure',
POSITIVE_RATIO_MEASURE(7850.),#12756);
#12863=MEASURE_REPRESENTATION_ITEM('density measure',
POSITIVE_RATIO_MEASURE(7850.),#12757);
#12864=MEASURE_REPRESENTATION_ITEM('density measure',
POSITIVE_RATIO_MEASURE(7850.),#12758);
#12865=MEASURE_REPRESENTATION_ITEM('density measure',
POSITIVE_RATIO_MEASURE(7850.),#12759);
#12866=MEASURE_REPRESENTATION_ITEM('density measure',
POSITIVE_RATIO_MEASURE(7850.),#12760);
#12867=MEASURE_REPRESENTATION_ITEM('density measure',
POSITIVE_RATIO_MEASURE(7850.),#12761);
#12868=MEASURE_REPRESENTATION_ITEM('density measure',
POSITIVE_RATIO_MEASURE(7850.),#12762);
#12869=MEASURE_REPRESENTATION_ITEM('density measure',
POSITIVE_RATIO_MEASURE(7850.),#12763);
#12870=MEASURE_REPRESENTATION_ITEM('density measure',
POSITIVE_RATIO_MEASURE(7850.),#12764);
#12871=MEASURE_REPRESENTATION_ITEM('density measure',
POSITIVE_RATIO_MEASURE(7850.),#12765);
#12872=MEASURE_REPRESENTATION_ITEM('density measure',
POSITIVE_RATIO_MEASURE(7850.),#12766);
#12873=MEASURE_REPRESENTATION_ITEM('density measure',
POSITIVE_RATIO_MEASURE(7850.),#12767);
#12874=MEASURE_REPRESENTATION_ITEM('density measure',
POSITIVE_RATIO_MEASURE(7850.),#12768);
#12875=MEASURE_REPRESENTATION_ITEM('density measure',
POSITIVE_RATIO_MEASURE(7850.),#12769);
#12876=MEASURE_REPRESENTATION_ITEM('density measure',
POSITIVE_RATIO_MEASURE(7850.),#12770);
#12877=MEASURE_REPRESENTATION_ITEM('density measure',
POSITIVE_RATIO_MEASURE(7850.),#12771);
#12878=MEASURE_REPRESENTATION_ITEM('density measure',
POSITIVE_RATIO_MEASURE(7850.),#12772);
#12879=MEASURE_REPRESENTATION_ITEM('density measure',
POSITIVE_RATIO_MEASURE(7850.),#12773);
#12880=MEASURE_REPRESENTATION_ITEM('density measure',
POSITIVE_RATIO_MEASURE(7850.),#12774);
#12881=MEASURE_REPRESENTATION_ITEM('density measure',
POSITIVE_RATIO_MEASURE(7850.),#12775);
#12882=MEASURE_REPRESENTATION_ITEM('density measure',
POSITIVE_RATIO_MEASURE(7850.),#12776);
#12883=MEASURE_REPRESENTATION_ITEM('density measure',
POSITIVE_RATIO_MEASURE(7850.),#12777);
#12884=MEASURE_REPRESENTATION_ITEM('density measure',
POSITIVE_RATIO_MEASURE(7850.),#12778);
#12885=MEASURE_REPRESENTATION_ITEM('density measure',
POSITIVE_RATIO_MEASURE(7850.),#12779);
#12886=MEASURE_REPRESENTATION_ITEM('density measure',
POSITIVE_RATIO_MEASURE(7850.),#12780);
#12887=MEASURE_REPRESENTATION_ITEM('density measure',
POSITIVE_RATIO_MEASURE(7850.),#12781);
#12888=MEASURE_REPRESENTATION_ITEM('density measure',
POSITIVE_RATIO_MEASURE(7850.),#12782);
#12889=MEASURE_REPRESENTATION_ITEM('density measure',
POSITIVE_RATIO_MEASURE(7850.),#12783);
#12890=MEASURE_REPRESENTATION_ITEM('density measure',
POSITIVE_RATIO_MEASURE(7850.),#12784);
#12891=MEASURE_REPRESENTATION_ITEM('density measure',
POSITIVE_RATIO_MEASURE(7850.),#12785);
#12892=MEASURE_REPRESENTATION_ITEM('density measure',
POSITIVE_RATIO_MEASURE(7850.),#12786);
#12893=MEASURE_REPRESENTATION_ITEM('density measure',
POSITIVE_RATIO_MEASURE(7850.),#12787);
#12894=MEASURE_REPRESENTATION_ITEM('density measure',
POSITIVE_RATIO_MEASURE(7850.),#12788);
#12895=MEASURE_REPRESENTATION_ITEM('density measure',
POSITIVE_RATIO_MEASURE(7850.),#12789);
#12896=MEASURE_REPRESENTATION_ITEM('density measure',
POSITIVE_RATIO_MEASURE(7850.),#12790);
#12897=MEASURE_REPRESENTATION_ITEM('density measure',
POSITIVE_RATIO_MEASURE(7850.),#12791);
#12898=MEASURE_REPRESENTATION_ITEM('density measure',
POSITIVE_RATIO_MEASURE(7850.),#12792);
#12899=MEASURE_REPRESENTATION_ITEM('density measure',
POSITIVE_RATIO_MEASURE(7850.),#12793);
#12900=MEASURE_REPRESENTATION_ITEM('density measure',
POSITIVE_RATIO_MEASURE(7850.),#12794);
#12901=MEASURE_REPRESENTATION_ITEM('density measure',
POSITIVE_RATIO_MEASURE(7850.),#12795);
#12902=MEASURE_REPRESENTATION_ITEM('density measure',
POSITIVE_RATIO_MEASURE(7850.),#12796);
#12903=MEASURE_REPRESENTATION_ITEM('density measure',
POSITIVE_RATIO_MEASURE(7850.),#12797);
#12904=MEASURE_REPRESENTATION_ITEM('density measure',
POSITIVE_RATIO_MEASURE(7850.),#12798);
#12905=MEASURE_REPRESENTATION_ITEM('density measure',
POSITIVE_RATIO_MEASURE(7850.),#12799);
#12906=MEASURE_REPRESENTATION_ITEM('density measure',
POSITIVE_RATIO_MEASURE(7850.),#12800);
#12907=MEASURE_REPRESENTATION_ITEM('density measure',
POSITIVE_RATIO_MEASURE(7850.),#12801);
#12908=MEASURE_REPRESENTATION_ITEM('density measure',
POSITIVE_RATIO_MEASURE(7850.),#12802);
#12909=MEASURE_REPRESENTATION_ITEM('density measure',
POSITIVE_RATIO_MEASURE(7850.),#12803);
#12910=MEASURE_REPRESENTATION_ITEM('density measure',
POSITIVE_RATIO_MEASURE(7850.),#12804);
#12911=MEASURE_REPRESENTATION_ITEM('density measure',
POSITIVE_RATIO_MEASURE(7850.),#12805);
#12912=MEASURE_REPRESENTATION_ITEM('density measure',
POSITIVE_RATIO_MEASURE(7850.),#12806);
#12913=MEASURE_REPRESENTATION_ITEM('density measure',
POSITIVE_RATIO_MEASURE(7850.),#12807);
#12914=MEASURE_REPRESENTATION_ITEM('density measure',
POSITIVE_RATIO_MEASURE(7850.),#12808);
#12915=MEASURE_REPRESENTATION_ITEM('density measure',
POSITIVE_RATIO_MEASURE(7850.),#12809);
#12916=MEASURE_REPRESENTATION_ITEM('density measure',
POSITIVE_RATIO_MEASURE(7850.),#12810);
#12917=MEASURE_REPRESENTATION_ITEM('density measure',
POSITIVE_RATIO_MEASURE(7850.),#12811);
#12918=MEASURE_REPRESENTATION_ITEM('density measure',
POSITIVE_RATIO_MEASURE(7850.),#12812);
#12919=MEASURE_REPRESENTATION_ITEM('density measure',
POSITIVE_RATIO_MEASURE(7850.),#12813);
#12920=MEASURE_REPRESENTATION_ITEM('density measure',
POSITIVE_RATIO_MEASURE(7850.),#12814);
#12921=MEASURE_REPRESENTATION_ITEM('density measure',
POSITIVE_RATIO_MEASURE(7850.),#12815);
#12922=MEASURE_REPRESENTATION_ITEM('density measure',
POSITIVE_RATIO_MEASURE(7850.),#12816);
#12923=MEASURE_REPRESENTATION_ITEM('density measure',
POSITIVE_RATIO_MEASURE(7850.),#12817);
#12924=MEASURE_REPRESENTATION_ITEM('density measure',
POSITIVE_RATIO_MEASURE(7850.),#12818);
#12925=MEASURE_REPRESENTATION_ITEM('density measure',
POSITIVE_RATIO_MEASURE(7850.),#12819);
#12926=MEASURE_REPRESENTATION_ITEM('density measure',
POSITIVE_RATIO_MEASURE(7850.),#12820);
#12927=MEASURE_REPRESENTATION_ITEM('density measure',
POSITIVE_RATIO_MEASURE(7850.),#12821);
#12928=MEASURE_REPRESENTATION_ITEM('density measure',
POSITIVE_RATIO_MEASURE(7850.),#12822);
#12929=MEASURE_REPRESENTATION_ITEM('density measure',
POSITIVE_RATIO_MEASURE(7850.),#12823);
#12930=MEASURE_REPRESENTATION_ITEM('density measure',
POSITIVE_RATIO_MEASURE(7850.),#12824);
#12931=MEASURE_REPRESENTATION_ITEM('density measure',
POSITIVE_RATIO_MEASURE(7850.),#12825);
#12932=MEASURE_REPRESENTATION_ITEM('density measure',
POSITIVE_RATIO_MEASURE(7850.),#12826);
#12933=MEASURE_REPRESENTATION_ITEM('density measure',
POSITIVE_RATIO_MEASURE(7850.),#12827);
#12934=PROPERTY_DEFINITION_REPRESENTATION(#13464,#13146);
#12935=PROPERTY_DEFINITION_REPRESENTATION(#13465,#13147);
#12936=PROPERTY_DEFINITION_REPRESENTATION(#13466,#13148);
#12937=PROPERTY_DEFINITION_REPRESENTATION(#13467,#13149);
#12938=PROPERTY_DEFINITION_REPRESENTATION(#13468,#13150);
#12939=PROPERTY_DEFINITION_REPRESENTATION(#13469,#13151);
#12940=PROPERTY_DEFINITION_REPRESENTATION(#13470,#13152);
#12941=PROPERTY_DEFINITION_REPRESENTATION(#13471,#13153);
#12942=PROPERTY_DEFINITION_REPRESENTATION(#13472,#13154);
#12943=PROPERTY_DEFINITION_REPRESENTATION(#13473,#13155);
#12944=PROPERTY_DEFINITION_REPRESENTATION(#13474,#13156);
#12945=PROPERTY_DEFINITION_REPRESENTATION(#13475,#13157);
#12946=PROPERTY_DEFINITION_REPRESENTATION(#13476,#13158);
#12947=PROPERTY_DEFINITION_REPRESENTATION(#13477,#13159);
#12948=PROPERTY_DEFINITION_REPRESENTATION(#13478,#13160);
#12949=PROPERTY_DEFINITION_REPRESENTATION(#13479,#13161);
#12950=PROPERTY_DEFINITION_REPRESENTATION(#13480,#13162);
#12951=PROPERTY_DEFINITION_REPRESENTATION(#13481,#13163);
#12952=PROPERTY_DEFINITION_REPRESENTATION(#13482,#13164);
#12953=PROPERTY_DEFINITION_REPRESENTATION(#13483,#13165);
#12954=PROPERTY_DEFINITION_REPRESENTATION(#13484,#13166);
#12955=PROPERTY_DEFINITION_REPRESENTATION(#13485,#13167);
#12956=PROPERTY_DEFINITION_REPRESENTATION(#13486,#13168);
#12957=PROPERTY_DEFINITION_REPRESENTATION(#13487,#13169);
#12958=PROPERTY_DEFINITION_REPRESENTATION(#13488,#13170);
#12959=PROPERTY_DEFINITION_REPRESENTATION(#13489,#13171);
#12960=PROPERTY_DEFINITION_REPRESENTATION(#13490,#13172);
#12961=PROPERTY_DEFINITION_REPRESENTATION(#13491,#13173);
#12962=PROPERTY_DEFINITION_REPRESENTATION(#13492,#13174);
#12963=PROPERTY_DEFINITION_REPRESENTATION(#13493,#13175);
#12964=PROPERTY_DEFINITION_REPRESENTATION(#13494,#13176);
#12965=PROPERTY_DEFINITION_REPRESENTATION(#13495,#13177);
#12966=PROPERTY_DEFINITION_REPRESENTATION(#13496,#13178);
#12967=PROPERTY_DEFINITION_REPRESENTATION(#13497,#13179);
#12968=PROPERTY_DEFINITION_REPRESENTATION(#13498,#13180);
#12969=PROPERTY_DEFINITION_REPRESENTATION(#13499,#13181);
#12970=PROPERTY_DEFINITION_REPRESENTATION(#13500,#13182);
#12971=PROPERTY_DEFINITION_REPRESENTATION(#13501,#13183);
#12972=PROPERTY_DEFINITION_REPRESENTATION(#13502,#13184);
#12973=PROPERTY_DEFINITION_REPRESENTATION(#13503,#13185);
#12974=PROPERTY_DEFINITION_REPRESENTATION(#13504,#13186);
#12975=PROPERTY_DEFINITION_REPRESENTATION(#13505,#13187);
#12976=PROPERTY_DEFINITION_REPRESENTATION(#13506,#13188);
#12977=PROPERTY_DEFINITION_REPRESENTATION(#13507,#13189);
#12978=PROPERTY_DEFINITION_REPRESENTATION(#13508,#13190);
#12979=PROPERTY_DEFINITION_REPRESENTATION(#13509,#13191);
#12980=PROPERTY_DEFINITION_REPRESENTATION(#13510,#13192);
#12981=PROPERTY_DEFINITION_REPRESENTATION(#13511,#13193);
#12982=PROPERTY_DEFINITION_REPRESENTATION(#13512,#13194);
#12983=PROPERTY_DEFINITION_REPRESENTATION(#13513,#13195);
#12984=PROPERTY_DEFINITION_REPRESENTATION(#13514,#13196);
#12985=PROPERTY_DEFINITION_REPRESENTATION(#13515,#13197);
#12986=PROPERTY_DEFINITION_REPRESENTATION(#13516,#13198);
#12987=PROPERTY_DEFINITION_REPRESENTATION(#13517,#13199);
#12988=PROPERTY_DEFINITION_REPRESENTATION(#13518,#13200);
#12989=PROPERTY_DEFINITION_REPRESENTATION(#13519,#13201);
#12990=PROPERTY_DEFINITION_REPRESENTATION(#13520,#13202);
#12991=PROPERTY_DEFINITION_REPRESENTATION(#13521,#13203);
#12992=PROPERTY_DEFINITION_REPRESENTATION(#13522,#13204);
#12993=PROPERTY_DEFINITION_REPRESENTATION(#13523,#13205);
#12994=PROPERTY_DEFINITION_REPRESENTATION(#13524,#13206);
#12995=PROPERTY_DEFINITION_REPRESENTATION(#13525,#13207);
#12996=PROPERTY_DEFINITION_REPRESENTATION(#13526,#13208);
#12997=PROPERTY_DEFINITION_REPRESENTATION(#13527,#13209);
#12998=PROPERTY_DEFINITION_REPRESENTATION(#13528,#13210);
#12999=PROPERTY_DEFINITION_REPRESENTATION(#13529,#13211);
#13000=PROPERTY_DEFINITION_REPRESENTATION(#13530,#13212);
#13001=PROPERTY_DEFINITION_REPRESENTATION(#13531,#13213);
#13002=PROPERTY_DEFINITION_REPRESENTATION(#13532,#13214);
#13003=PROPERTY_DEFINITION_REPRESENTATION(#13533,#13215);
#13004=PROPERTY_DEFINITION_REPRESENTATION(#13534,#13216);
#13005=PROPERTY_DEFINITION_REPRESENTATION(#13535,#13217);
#13006=PROPERTY_DEFINITION_REPRESENTATION(#13536,#13218);
#13007=PROPERTY_DEFINITION_REPRESENTATION(#13537,#13219);
#13008=PROPERTY_DEFINITION_REPRESENTATION(#13538,#13220);
#13009=PROPERTY_DEFINITION_REPRESENTATION(#13539,#13221);
#13010=PROPERTY_DEFINITION_REPRESENTATION(#13540,#13222);
#13011=PROPERTY_DEFINITION_REPRESENTATION(#13541,#13223);
#13012=PROPERTY_DEFINITION_REPRESENTATION(#13542,#13224);
#13013=PROPERTY_DEFINITION_REPRESENTATION(#13543,#13225);
#13014=PROPERTY_DEFINITION_REPRESENTATION(#13544,#13226);
#13015=PROPERTY_DEFINITION_REPRESENTATION(#13545,#13227);
#13016=PROPERTY_DEFINITION_REPRESENTATION(#13546,#13228);
#13017=PROPERTY_DEFINITION_REPRESENTATION(#13547,#13229);
#13018=PROPERTY_DEFINITION_REPRESENTATION(#13548,#13230);
#13019=PROPERTY_DEFINITION_REPRESENTATION(#13549,#13231);
#13020=PROPERTY_DEFINITION_REPRESENTATION(#13550,#13232);
#13021=PROPERTY_DEFINITION_REPRESENTATION(#13551,#13233);
#13022=PROPERTY_DEFINITION_REPRESENTATION(#13552,#13234);
#13023=PROPERTY_DEFINITION_REPRESENTATION(#13553,#13235);
#13024=PROPERTY_DEFINITION_REPRESENTATION(#13554,#13236);
#13025=PROPERTY_DEFINITION_REPRESENTATION(#13555,#13237);
#13026=PROPERTY_DEFINITION_REPRESENTATION(#13556,#13238);
#13027=PROPERTY_DEFINITION_REPRESENTATION(#13557,#13239);
#13028=PROPERTY_DEFINITION_REPRESENTATION(#13558,#13240);
#13029=PROPERTY_DEFINITION_REPRESENTATION(#13559,#13241);
#13030=PROPERTY_DEFINITION_REPRESENTATION(#13560,#13242);
#13031=PROPERTY_DEFINITION_REPRESENTATION(#13561,#13243);
#13032=PROPERTY_DEFINITION_REPRESENTATION(#13562,#13244);
#13033=PROPERTY_DEFINITION_REPRESENTATION(#13563,#13245);
#13034=PROPERTY_DEFINITION_REPRESENTATION(#13564,#13246);
#13035=PROPERTY_DEFINITION_REPRESENTATION(#13565,#13247);
#13036=PROPERTY_DEFINITION_REPRESENTATION(#13566,#13248);
#13037=PROPERTY_DEFINITION_REPRESENTATION(#13567,#13249);
#13038=PROPERTY_DEFINITION_REPRESENTATION(#13568,#13250);
#13039=PROPERTY_DEFINITION_REPRESENTATION(#13569,#13251);
#13040=PROPERTY_DEFINITION_REPRESENTATION(#13570,#13252);
#13041=PROPERTY_DEFINITION_REPRESENTATION(#13571,#13253);
#13042=PROPERTY_DEFINITION_REPRESENTATION(#13572,#13254);
#13043=PROPERTY_DEFINITION_REPRESENTATION(#13573,#13255);
#13044=PROPERTY_DEFINITION_REPRESENTATION(#13574,#13256);
#13045=PROPERTY_DEFINITION_REPRESENTATION(#13575,#13257);
#13046=PROPERTY_DEFINITION_REPRESENTATION(#13576,#13258);
#13047=PROPERTY_DEFINITION_REPRESENTATION(#13577,#13259);
#13048=PROPERTY_DEFINITION_REPRESENTATION(#13578,#13260);
#13049=PROPERTY_DEFINITION_REPRESENTATION(#13579,#13261);
#13050=PROPERTY_DEFINITION_REPRESENTATION(#13580,#13262);
#13051=PROPERTY_DEFINITION_REPRESENTATION(#13581,#13263);
#13052=PROPERTY_DEFINITION_REPRESENTATION(#13582,#13264);
#13053=PROPERTY_DEFINITION_REPRESENTATION(#13583,#13265);
#13054=PROPERTY_DEFINITION_REPRESENTATION(#13584,#13266);
#13055=PROPERTY_DEFINITION_REPRESENTATION(#13585,#13267);
#13056=PROPERTY_DEFINITION_REPRESENTATION(#13586,#13268);
#13057=PROPERTY_DEFINITION_REPRESENTATION(#13587,#13269);
#13058=PROPERTY_DEFINITION_REPRESENTATION(#13588,#13270);
#13059=PROPERTY_DEFINITION_REPRESENTATION(#13589,#13271);
#13060=PROPERTY_DEFINITION_REPRESENTATION(#13590,#13272);
#13061=PROPERTY_DEFINITION_REPRESENTATION(#13591,#13273);
#13062=PROPERTY_DEFINITION_REPRESENTATION(#13592,#13274);
#13063=PROPERTY_DEFINITION_REPRESENTATION(#13593,#13275);
#13064=PROPERTY_DEFINITION_REPRESENTATION(#13594,#13276);
#13065=PROPERTY_DEFINITION_REPRESENTATION(#13595,#13277);
#13066=PROPERTY_DEFINITION_REPRESENTATION(#13596,#13278);
#13067=PROPERTY_DEFINITION_REPRESENTATION(#13597,#13279);
#13068=PROPERTY_DEFINITION_REPRESENTATION(#13598,#13280);
#13069=PROPERTY_DEFINITION_REPRESENTATION(#13599,#13281);
#13070=PROPERTY_DEFINITION_REPRESENTATION(#13600,#13282);
#13071=PROPERTY_DEFINITION_REPRESENTATION(#13601,#13283);
#13072=PROPERTY_DEFINITION_REPRESENTATION(#13602,#13284);
#13073=PROPERTY_DEFINITION_REPRESENTATION(#13603,#13285);
#13074=PROPERTY_DEFINITION_REPRESENTATION(#13604,#13286);
#13075=PROPERTY_DEFINITION_REPRESENTATION(#13605,#13287);
#13076=PROPERTY_DEFINITION_REPRESENTATION(#13606,#13288);
#13077=PROPERTY_DEFINITION_REPRESENTATION(#13607,#13289);
#13078=PROPERTY_DEFINITION_REPRESENTATION(#13608,#13290);
#13079=PROPERTY_DEFINITION_REPRESENTATION(#13609,#13291);
#13080=PROPERTY_DEFINITION_REPRESENTATION(#13610,#13292);
#13081=PROPERTY_DEFINITION_REPRESENTATION(#13611,#13293);
#13082=PROPERTY_DEFINITION_REPRESENTATION(#13612,#13294);
#13083=PROPERTY_DEFINITION_REPRESENTATION(#13613,#13295);
#13084=PROPERTY_DEFINITION_REPRESENTATION(#13614,#13296);
#13085=PROPERTY_DEFINITION_REPRESENTATION(#13615,#13297);
#13086=PROPERTY_DEFINITION_REPRESENTATION(#13616,#13298);
#13087=PROPERTY_DEFINITION_REPRESENTATION(#13617,#13299);
#13088=PROPERTY_DEFINITION_REPRESENTATION(#13618,#13300);
#13089=PROPERTY_DEFINITION_REPRESENTATION(#13619,#13301);
#13090=PROPERTY_DEFINITION_REPRESENTATION(#13620,#13302);
#13091=PROPERTY_DEFINITION_REPRESENTATION(#13621,#13303);
#13092=PROPERTY_DEFINITION_REPRESENTATION(#13622,#13304);
#13093=PROPERTY_DEFINITION_REPRESENTATION(#13623,#13305);
#13094=PROPERTY_DEFINITION_REPRESENTATION(#13624,#13306);
#13095=PROPERTY_DEFINITION_REPRESENTATION(#13625,#13307);
#13096=PROPERTY_DEFINITION_REPRESENTATION(#13626,#13308);
#13097=PROPERTY_DEFINITION_REPRESENTATION(#13627,#13309);
#13098=PROPERTY_DEFINITION_REPRESENTATION(#13628,#13310);
#13099=PROPERTY_DEFINITION_REPRESENTATION(#13629,#13311);
#13100=PROPERTY_DEFINITION_REPRESENTATION(#13630,#13312);
#13101=PROPERTY_DEFINITION_REPRESENTATION(#13631,#13313);
#13102=PROPERTY_DEFINITION_REPRESENTATION(#13632,#13314);
#13103=PROPERTY_DEFINITION_REPRESENTATION(#13633,#13315);
#13104=PROPERTY_DEFINITION_REPRESENTATION(#13634,#13316);
#13105=PROPERTY_DEFINITION_REPRESENTATION(#13635,#13317);
#13106=PROPERTY_DEFINITION_REPRESENTATION(#13636,#13318);
#13107=PROPERTY_DEFINITION_REPRESENTATION(#13637,#13319);
#13108=PROPERTY_DEFINITION_REPRESENTATION(#13638,#13320);
#13109=PROPERTY_DEFINITION_REPRESENTATION(#13639,#13321);
#13110=PROPERTY_DEFINITION_REPRESENTATION(#13640,#13322);
#13111=PROPERTY_DEFINITION_REPRESENTATION(#13641,#13323);
#13112=PROPERTY_DEFINITION_REPRESENTATION(#13642,#13324);
#13113=PROPERTY_DEFINITION_REPRESENTATION(#13643,#13325);
#13114=PROPERTY_DEFINITION_REPRESENTATION(#13644,#13326);
#13115=PROPERTY_DEFINITION_REPRESENTATION(#13645,#13327);
#13116=PROPERTY_DEFINITION_REPRESENTATION(#13646,#13328);
#13117=PROPERTY_DEFINITION_REPRESENTATION(#13647,#13329);
#13118=PROPERTY_DEFINITION_REPRESENTATION(#13648,#13330);
#13119=PROPERTY_DEFINITION_REPRESENTATION(#13649,#13331);
#13120=PROPERTY_DEFINITION_REPRESENTATION(#13650,#13332);
#13121=PROPERTY_DEFINITION_REPRESENTATION(#13651,#13333);
#13122=PROPERTY_DEFINITION_REPRESENTATION(#13652,#13334);
#13123=PROPERTY_DEFINITION_REPRESENTATION(#13653,#13335);
#13124=PROPERTY_DEFINITION_REPRESENTATION(#13654,#13336);
#13125=PROPERTY_DEFINITION_REPRESENTATION(#13655,#13337);
#13126=PROPERTY_DEFINITION_REPRESENTATION(#13656,#13338);
#13127=PROPERTY_DEFINITION_REPRESENTATION(#13657,#13339);
#13128=PROPERTY_DEFINITION_REPRESENTATION(#13658,#13340);
#13129=PROPERTY_DEFINITION_REPRESENTATION(#13659,#13341);
#13130=PROPERTY_DEFINITION_REPRESENTATION(#13660,#13342);
#13131=PROPERTY_DEFINITION_REPRESENTATION(#13661,#13343);
#13132=PROPERTY_DEFINITION_REPRESENTATION(#13662,#13344);
#13133=PROPERTY_DEFINITION_REPRESENTATION(#13663,#13345);
#13134=PROPERTY_DEFINITION_REPRESENTATION(#13664,#13346);
#13135=PROPERTY_DEFINITION_REPRESENTATION(#13665,#13347);
#13136=PROPERTY_DEFINITION_REPRESENTATION(#13666,#13348);
#13137=PROPERTY_DEFINITION_REPRESENTATION(#13667,#13349);
#13138=PROPERTY_DEFINITION_REPRESENTATION(#13668,#13350);
#13139=PROPERTY_DEFINITION_REPRESENTATION(#13669,#13351);
#13140=PROPERTY_DEFINITION_REPRESENTATION(#13670,#13352);
#13141=PROPERTY_DEFINITION_REPRESENTATION(#13671,#13353);
#13142=PROPERTY_DEFINITION_REPRESENTATION(#13672,#13354);
#13143=PROPERTY_DEFINITION_REPRESENTATION(#13673,#13355);
#13144=PROPERTY_DEFINITION_REPRESENTATION(#13674,#13356);
#13145=PROPERTY_DEFINITION_REPRESENTATION(#13675,#13357);
#13146=REPRESENTATION('material name',(#13358),#23614);
#13147=REPRESENTATION('density',(#12828),#23614);
#13148=REPRESENTATION('material name',(#13359),#23615);
#13149=REPRESENTATION('density',(#12829),#23615);
#13150=REPRESENTATION('material name',(#13360),#23616);
#13151=REPRESENTATION('density',(#12830),#23616);
#13152=REPRESENTATION('material name',(#13361),#23617);
#13153=REPRESENTATION('density',(#12831),#23617);
#13154=REPRESENTATION('material name',(#13362),#23618);
#13155=REPRESENTATION('density',(#12832),#23618);
#13156=REPRESENTATION('material name',(#13363),#23619);
#13157=REPRESENTATION('density',(#12833),#23619);
#13158=REPRESENTATION('material name',(#13364),#23620);
#13159=REPRESENTATION('density',(#12834),#23620);
#13160=REPRESENTATION('material name',(#13365),#23621);
#13161=REPRESENTATION('density',(#12835),#23621);
#13162=REPRESENTATION('material name',(#13366),#23622);
#13163=REPRESENTATION('density',(#12836),#23622);
#13164=REPRESENTATION('material name',(#13367),#23623);
#13165=REPRESENTATION('density',(#12837),#23623);
#13166=REPRESENTATION('material name',(#13368),#23624);
#13167=REPRESENTATION('density',(#12838),#23624);
#13168=REPRESENTATION('material name',(#13369),#23625);
#13169=REPRESENTATION('density',(#12839),#23625);
#13170=REPRESENTATION('material name',(#13370),#23626);
#13171=REPRESENTATION('density',(#12840),#23626);
#13172=REPRESENTATION('material name',(#13371),#23627);
#13173=REPRESENTATION('density',(#12841),#23627);
#13174=REPRESENTATION('material name',(#13372),#23628);
#13175=REPRESENTATION('density',(#12842),#23628);
#13176=REPRESENTATION('material name',(#13373),#23629);
#13177=REPRESENTATION('density',(#12843),#23629);
#13178=REPRESENTATION('material name',(#13374),#23630);
#13179=REPRESENTATION('density',(#12844),#23630);
#13180=REPRESENTATION('material name',(#13375),#23631);
#13181=REPRESENTATION('density',(#12845),#23631);
#13182=REPRESENTATION('material name',(#13376),#23632);
#13183=REPRESENTATION('density',(#12846),#23632);
#13184=REPRESENTATION('material name',(#13377),#23633);
#13185=REPRESENTATION('density',(#12847),#23633);
#13186=REPRESENTATION('material name',(#13378),#23634);
#13187=REPRESENTATION('density',(#12848),#23634);
#13188=REPRESENTATION('material name',(#13379),#23635);
#13189=REPRESENTATION('density',(#12849),#23635);
#13190=REPRESENTATION('material name',(#13380),#23636);
#13191=REPRESENTATION('density',(#12850),#23636);
#13192=REPRESENTATION('material name',(#13381),#23637);
#13193=REPRESENTATION('density',(#12851),#23637);
#13194=REPRESENTATION('material name',(#13382),#23638);
#13195=REPRESENTATION('density',(#12852),#23638);
#13196=REPRESENTATION('material name',(#13383),#23639);
#13197=REPRESENTATION('density',(#12853),#23639);
#13198=REPRESENTATION('material name',(#13384),#23640);
#13199=REPRESENTATION('density',(#12854),#23640);
#13200=REPRESENTATION('material name',(#13385),#23641);
#13201=REPRESENTATION('density',(#12855),#23641);
#13202=REPRESENTATION('material name',(#13386),#23642);
#13203=REPRESENTATION('density',(#12856),#23642);
#13204=REPRESENTATION('material name',(#13387),#23643);
#13205=REPRESENTATION('density',(#12857),#23643);
#13206=REPRESENTATION('material name',(#13388),#23645);
#13207=REPRESENTATION('density',(#12858),#23645);
#13208=REPRESENTATION('material name',(#13389),#23646);
#13209=REPRESENTATION('density',(#12859),#23646);
#13210=REPRESENTATION('material name',(#13390),#23647);
#13211=REPRESENTATION('density',(#12860),#23647);
#13212=REPRESENTATION('material name',(#13391),#23648);
#13213=REPRESENTATION('density',(#12861),#23648);
#13214=REPRESENTATION('material name',(#13392),#23649);
#13215=REPRESENTATION('density',(#12862),#23649);
#13216=REPRESENTATION('material name',(#13393),#23650);
#13217=REPRESENTATION('density',(#12863),#23650);
#13218=REPRESENTATION('material name',(#13394),#23651);
#13219=REPRESENTATION('density',(#12864),#23651);
#13220=REPRESENTATION('material name',(#13395),#23652);
#13221=REPRESENTATION('density',(#12865),#23652);
#13222=REPRESENTATION('material name',(#13396),#23653);
#13223=REPRESENTATION('density',(#12866),#23653);
#13224=REPRESENTATION('material name',(#13397),#23654);
#13225=REPRESENTATION('density',(#12867),#23654);
#13226=REPRESENTATION('material name',(#13398),#23655);
#13227=REPRESENTATION('density',(#12868),#23655);
#13228=REPRESENTATION('material name',(#13399),#23656);
#13229=REPRESENTATION('density',(#12869),#23656);
#13230=REPRESENTATION('material name',(#13400),#23657);
#13231=REPRESENTATION('density',(#12870),#23657);
#13232=REPRESENTATION('material name',(#13401),#23658);
#13233=REPRESENTATION('density',(#12871),#23658);
#13234=REPRESENTATION('material name',(#13402),#23659);
#13235=REPRESENTATION('density',(#12872),#23659);
#13236=REPRESENTATION('material name',(#13403),#23660);
#13237=REPRESENTATION('density',(#12873),#23660);
#13238=REPRESENTATION('material name',(#13404),#23661);
#13239=REPRESENTATION('density',(#12874),#23661);
#13240=REPRESENTATION('material name',(#13405),#23662);
#13241=REPRESENTATION('density',(#12875),#23662);
#13242=REPRESENTATION('material name',(#13406),#23663);
#13243=REPRESENTATION('density',(#12876),#23663);
#13244=REPRESENTATION('material name',(#13407),#23664);
#13245=REPRESENTATION('density',(#12877),#23664);
#13246=REPRESENTATION('material name',(#13408),#23665);
#13247=REPRESENTATION('density',(#12878),#23665);
#13248=REPRESENTATION('material name',(#13409),#23667);
#13249=REPRESENTATION('density',(#12879),#23667);
#13250=REPRESENTATION('material name',(#13410),#23668);
#13251=REPRESENTATION('density',(#12880),#23668);
#13252=REPRESENTATION('material name',(#13411),#23669);
#13253=REPRESENTATION('density',(#12881),#23669);
#13254=REPRESENTATION('material name',(#13412),#23670);
#13255=REPRESENTATION('density',(#12882),#23670);
#13256=REPRESENTATION('material name',(#13413),#23671);
#13257=REPRESENTATION('density',(#12883),#23671);
#13258=REPRESENTATION('material name',(#13414),#23672);
#13259=REPRESENTATION('density',(#12884),#23672);
#13260=REPRESENTATION('material name',(#13415),#23673);
#13261=REPRESENTATION('density',(#12885),#23673);
#13262=REPRESENTATION('material name',(#13416),#23674);
#13263=REPRESENTATION('density',(#12886),#23674);
#13264=REPRESENTATION('material name',(#13417),#23675);
#13265=REPRESENTATION('density',(#12887),#23675);
#13266=REPRESENTATION('material name',(#13418),#23676);
#13267=REPRESENTATION('density',(#12888),#23676);
#13268=REPRESENTATION('material name',(#13419),#23677);
#13269=REPRESENTATION('density',(#12889),#23677);
#13270=REPRESENTATION('material name',(#13420),#23678);
#13271=REPRESENTATION('density',(#12890),#23678);
#13272=REPRESENTATION('material name',(#13421),#23679);
#13273=REPRESENTATION('density',(#12891),#23679);
#13274=REPRESENTATION('material name',(#13422),#23680);
#13275=REPRESENTATION('density',(#12892),#23680);
#13276=REPRESENTATION('material name',(#13423),#23681);
#13277=REPRESENTATION('density',(#12893),#23681);
#13278=REPRESENTATION('material name',(#13424),#23682);
#13279=REPRESENTATION('density',(#12894),#23682);
#13280=REPRESENTATION('material name',(#13425),#23683);
#13281=REPRESENTATION('density',(#12895),#23683);
#13282=REPRESENTATION('material name',(#13426),#23684);
#13283=REPRESENTATION('density',(#12896),#23684);
#13284=REPRESENTATION('material name',(#13427),#23685);
#13285=REPRESENTATION('density',(#12897),#23685);
#13286=REPRESENTATION('material name',(#13428),#23686);
#13287=REPRESENTATION('density',(#12898),#23686);
#13288=REPRESENTATION('material name',(#13429),#23687);
#13289=REPRESENTATION('density',(#12899),#23687);
#13290=REPRESENTATION('material name',(#13430),#23689);
#13291=REPRESENTATION('density',(#12900),#23689);
#13292=REPRESENTATION('material name',(#13431),#23690);
#13293=REPRESENTATION('density',(#12901),#23690);
#13294=REPRESENTATION('material name',(#13432),#23691);
#13295=REPRESENTATION('density',(#12902),#23691);
#13296=REPRESENTATION('material name',(#13433),#23692);
#13297=REPRESENTATION('density',(#12903),#23692);
#13298=REPRESENTATION('material name',(#13434),#23693);
#13299=REPRESENTATION('density',(#12904),#23693);
#13300=REPRESENTATION('material name',(#13435),#23695);
#13301=REPRESENTATION('density',(#12905),#23695);
#13302=REPRESENTATION('material name',(#13436),#23696);
#13303=REPRESENTATION('density',(#12906),#23696);
#13304=REPRESENTATION('material name',(#13437),#23697);
#13305=REPRESENTATION('density',(#12907),#23697);
#13306=REPRESENTATION('material name',(#13438),#23698);
#13307=REPRESENTATION('density',(#12908),#23698);
#13308=REPRESENTATION('material name',(#13439),#23699);
#13309=REPRESENTATION('density',(#12909),#23699);
#13310=REPRESENTATION('material name',(#13440),#23700);
#13311=REPRESENTATION('density',(#12910),#23700);
#13312=REPRESENTATION('material name',(#13441),#23701);
#13313=REPRESENTATION('density',(#12911),#23701);
#13314=REPRESENTATION('material name',(#13442),#23702);
#13315=REPRESENTATION('density',(#12912),#23702);
#13316=REPRESENTATION('material name',(#13443),#23703);
#13317=REPRESENTATION('density',(#12913),#23703);
#13318=REPRESENTATION('material name',(#13444),#23704);
#13319=REPRESENTATION('density',(#12914),#23704);
#13320=REPRESENTATION('material name',(#13445),#23705);
#13321=REPRESENTATION('density',(#12915),#23705);
#13322=REPRESENTATION('material name',(#13446),#23706);
#13323=REPRESENTATION('density',(#12916),#23706);
#13324=REPRESENTATION('material name',(#13447),#23707);
#13325=REPRESENTATION('density',(#12917),#23707);
#13326=REPRESENTATION('material name',(#13448),#23709);
#13327=REPRESENTATION('density',(#12918),#23709);
#13328=REPRESENTATION('material name',(#13449),#23710);
#13329=REPRESENTATION('density',(#12919),#23710);
#13330=REPRESENTATION('material name',(#13450),#23711);
#13331=REPRESENTATION('density',(#12920),#23711);
#13332=REPRESENTATION('material name',(#13451),#23712);
#13333=REPRESENTATION('density',(#12921),#23712);
#13334=REPRESENTATION('material name',(#13452),#23713);
#13335=REPRESENTATION('density',(#12922),#23713);
#13336=REPRESENTATION('material name',(#13453),#23714);
#13337=REPRESENTATION('density',(#12923),#23714);
#13338=REPRESENTATION('material name',(#13454),#23715);
#13339=REPRESENTATION('density',(#12924),#23715);
#13340=REPRESENTATION('material name',(#13455),#23717);
#13341=REPRESENTATION('density',(#12925),#23717);
#13342=REPRESENTATION('material name',(#13456),#23718);
#13343=REPRESENTATION('density',(#12926),#23718);
#13344=REPRESENTATION('material name',(#13457),#23719);
#13345=REPRESENTATION('density',(#12927),#23719);
#13346=REPRESENTATION('material name',(#13458),#23721);
#13347=REPRESENTATION('density',(#12928),#23721);
#13348=REPRESENTATION('material name',(#13459),#23723);
#13349=REPRESENTATION('density',(#12929),#23723);
#13350=REPRESENTATION('material name',(#13460),#23724);
#13351=REPRESENTATION('density',(#12930),#23724);
#13352=REPRESENTATION('material name',(#13461),#23725);
#13353=REPRESENTATION('density',(#12931),#23725);
#13354=REPRESENTATION('material name',(#13462),#23726);
#13355=REPRESENTATION('density',(#12932),#23726);
#13356=REPRESENTATION('material name',(#13463),#23727);
#13357=REPRESENTATION('density',(#12933),#23727);
#13358=DESCRIPTIVE_REPRESENTATION_ITEM('Steel','Steel');
#13359=DESCRIPTIVE_REPRESENTATION_ITEM('Steel','Steel');
#13360=DESCRIPTIVE_REPRESENTATION_ITEM('Steel','Steel');
#13361=DESCRIPTIVE_REPRESENTATION_ITEM('Steel','Steel');
#13362=DESCRIPTIVE_REPRESENTATION_ITEM('Steel','Steel');
#13363=DESCRIPTIVE_REPRESENTATION_ITEM('Steel','Steel');
#13364=DESCRIPTIVE_REPRESENTATION_ITEM('Steel','Steel');
#13365=DESCRIPTIVE_REPRESENTATION_ITEM('Steel','Steel');
#13366=DESCRIPTIVE_REPRESENTATION_ITEM('Steel','Steel');
#13367=DESCRIPTIVE_REPRESENTATION_ITEM('Steel','Steel');
#13368=DESCRIPTIVE_REPRESENTATION_ITEM('Steel','Steel');
#13369=DESCRIPTIVE_REPRESENTATION_ITEM('Steel','Steel');
#13370=DESCRIPTIVE_REPRESENTATION_ITEM('Steel','Steel');
#13371=DESCRIPTIVE_REPRESENTATION_ITEM('Steel','Steel');
#13372=DESCRIPTIVE_REPRESENTATION_ITEM('Steel','Steel');
#13373=DESCRIPTIVE_REPRESENTATION_ITEM('Steel','Steel');
#13374=DESCRIPTIVE_REPRESENTATION_ITEM('Steel','Steel');
#13375=DESCRIPTIVE_REPRESENTATION_ITEM('Steel','Steel');
#13376=DESCRIPTIVE_REPRESENTATION_ITEM('Steel','Steel');
#13377=DESCRIPTIVE_REPRESENTATION_ITEM('Steel','Steel');
#13378=DESCRIPTIVE_REPRESENTATION_ITEM('Steel','Steel');
#13379=DESCRIPTIVE_REPRESENTATION_ITEM('Steel','Steel');
#13380=DESCRIPTIVE_REPRESENTATION_ITEM('Steel','Steel');
#13381=DESCRIPTIVE_REPRESENTATION_ITEM('Steel','Steel');
#13382=DESCRIPTIVE_REPRESENTATION_ITEM('Steel','Steel');
#13383=DESCRIPTIVE_REPRESENTATION_ITEM('Steel','Steel');
#13384=DESCRIPTIVE_REPRESENTATION_ITEM('Steel','Steel');
#13385=DESCRIPTIVE_REPRESENTATION_ITEM('Steel','Steel');
#13386=DESCRIPTIVE_REPRESENTATION_ITEM('Steel','Steel');
#13387=DESCRIPTIVE_REPRESENTATION_ITEM('Steel','Steel');
#13388=DESCRIPTIVE_REPRESENTATION_ITEM('Steel','Steel');
#13389=DESCRIPTIVE_REPRESENTATION_ITEM('Steel','Steel');
#13390=DESCRIPTIVE_REPRESENTATION_ITEM('Steel','Steel');
#13391=DESCRIPTIVE_REPRESENTATION_ITEM('Steel','Steel');
#13392=DESCRIPTIVE_REPRESENTATION_ITEM('Steel','Steel');
#13393=DESCRIPTIVE_REPRESENTATION_ITEM('Steel','Steel');
#13394=DESCRIPTIVE_REPRESENTATION_ITEM('Steel','Steel');
#13395=DESCRIPTIVE_REPRESENTATION_ITEM('Steel','Steel');
#13396=DESCRIPTIVE_REPRESENTATION_ITEM('Steel','Steel');
#13397=DESCRIPTIVE_REPRESENTATION_ITEM('Steel','Steel');
#13398=DESCRIPTIVE_REPRESENTATION_ITEM('Steel','Steel');
#13399=DESCRIPTIVE_REPRESENTATION_ITEM('Steel','Steel');
#13400=DESCRIPTIVE_REPRESENTATION_ITEM('Steel','Steel');
#13401=DESCRIPTIVE_REPRESENTATION_ITEM('Steel','Steel');
#13402=DESCRIPTIVE_REPRESENTATION_ITEM('Steel','Steel');
#13403=DESCRIPTIVE_REPRESENTATION_ITEM('Steel','Steel');
#13404=DESCRIPTIVE_REPRESENTATION_ITEM('Steel','Steel');
#13405=DESCRIPTIVE_REPRESENTATION_ITEM('Steel','Steel');
#13406=DESCRIPTIVE_REPRESENTATION_ITEM('Steel','Steel');
#13407=DESCRIPTIVE_REPRESENTATION_ITEM('Steel','Steel');
#13408=DESCRIPTIVE_REPRESENTATION_ITEM('Steel','Steel');
#13409=DESCRIPTIVE_REPRESENTATION_ITEM('Steel','Steel');
#13410=DESCRIPTIVE_REPRESENTATION_ITEM('Steel','Steel');
#13411=DESCRIPTIVE_REPRESENTATION_ITEM('Steel','Steel');
#13412=DESCRIPTIVE_REPRESENTATION_ITEM('Steel','Steel');
#13413=DESCRIPTIVE_REPRESENTATION_ITEM('Steel','Steel');
#13414=DESCRIPTIVE_REPRESENTATION_ITEM('Steel','Steel');
#13415=DESCRIPTIVE_REPRESENTATION_ITEM('Steel','Steel');
#13416=DESCRIPTIVE_REPRESENTATION_ITEM('Steel','Steel');
#13417=DESCRIPTIVE_REPRESENTATION_ITEM('Steel','Steel');
#13418=DESCRIPTIVE_REPRESENTATION_ITEM('Steel','Steel');
#13419=DESCRIPTIVE_REPRESENTATION_ITEM('Steel','Steel');
#13420=DESCRIPTIVE_REPRESENTATION_ITEM('Steel','Steel');
#13421=DESCRIPTIVE_REPRESENTATION_ITEM('Steel','Steel');
#13422=DESCRIPTIVE_REPRESENTATION_ITEM('Steel','Steel');
#13423=DESCRIPTIVE_REPRESENTATION_ITEM('Steel','Steel');
#13424=DESCRIPTIVE_REPRESENTATION_ITEM('Steel','Steel');
#13425=DESCRIPTIVE_REPRESENTATION_ITEM('Steel','Steel');
#13426=DESCRIPTIVE_REPRESENTATION_ITEM('Steel','Steel');
#13427=DESCRIPTIVE_REPRESENTATION_ITEM('Steel','Steel');
#13428=DESCRIPTIVE_REPRESENTATION_ITEM('Steel','Steel');
#13429=DESCRIPTIVE_REPRESENTATION_ITEM('Steel','Steel');
#13430=DESCRIPTIVE_REPRESENTATION_ITEM('Steel','Steel');
#13431=DESCRIPTIVE_REPRESENTATION_ITEM('Steel','Steel');
#13432=DESCRIPTIVE_REPRESENTATION_ITEM('Steel','Steel');
#13433=DESCRIPTIVE_REPRESENTATION_ITEM('Steel','Steel');
#13434=DESCRIPTIVE_REPRESENTATION_ITEM('Steel','Steel');
#13435=DESCRIPTIVE_REPRESENTATION_ITEM('Steel','Steel');
#13436=DESCRIPTIVE_REPRESENTATION_ITEM('Steel','Steel');
#13437=DESCRIPTIVE_REPRESENTATION_ITEM('Steel','Steel');
#13438=DESCRIPTIVE_REPRESENTATION_ITEM('Steel','Steel');
#13439=DESCRIPTIVE_REPRESENTATION_ITEM('Steel','Steel');
#13440=DESCRIPTIVE_REPRESENTATION_ITEM('Steel','Steel');
#13441=DESCRIPTIVE_REPRESENTATION_ITEM('Steel','Steel');
#13442=DESCRIPTIVE_REPRESENTATION_ITEM('Steel','Steel');
#13443=DESCRIPTIVE_REPRESENTATION_ITEM('Steel','Steel');
#13444=DESCRIPTIVE_REPRESENTATION_ITEM('Steel','Steel');
#13445=DESCRIPTIVE_REPRESENTATION_ITEM('Steel','Steel');
#13446=DESCRIPTIVE_REPRESENTATION_ITEM('Steel','Steel');
#13447=DESCRIPTIVE_REPRESENTATION_ITEM('Steel','Steel');
#13448=DESCRIPTIVE_REPRESENTATION_ITEM('Steel','Steel');
#13449=DESCRIPTIVE_REPRESENTATION_ITEM('Steel','Steel');
#13450=DESCRIPTIVE_REPRESENTATION_ITEM('Steel','Steel');
#13451=DESCRIPTIVE_REPRESENTATION_ITEM('Steel','Steel');
#13452=DESCRIPTIVE_REPRESENTATION_ITEM('Steel','Steel');
#13453=DESCRIPTIVE_REPRESENTATION_ITEM('Steel','Steel');
#13454=DESCRIPTIVE_REPRESENTATION_ITEM('Steel','Steel');
#13455=DESCRIPTIVE_REPRESENTATION_ITEM('Steel','Steel');
#13456=DESCRIPTIVE_REPRESENTATION_ITEM('Steel','Steel');
#13457=DESCRIPTIVE_REPRESENTATION_ITEM('Steel','Steel');
#13458=DESCRIPTIVE_REPRESENTATION_ITEM('Steel','Steel');
#13459=DESCRIPTIVE_REPRESENTATION_ITEM('Steel','Steel');
#13460=DESCRIPTIVE_REPRESENTATION_ITEM('Steel','Steel');
#13461=DESCRIPTIVE_REPRESENTATION_ITEM('Steel','Steel');
#13462=DESCRIPTIVE_REPRESENTATION_ITEM('Steel','Steel');
#13463=DESCRIPTIVE_REPRESENTATION_ITEM('Steel','Steel');
#13464=PROPERTY_DEFINITION('material property','material name',#24231);
#13465=PROPERTY_DEFINITION('material property','density of part',#24231);
#13466=PROPERTY_DEFINITION('material property','material name',#24232);
#13467=PROPERTY_DEFINITION('material property','density of part',#24232);
#13468=PROPERTY_DEFINITION('material property','material name',#24233);
#13469=PROPERTY_DEFINITION('material property','density of part',#24233);
#13470=PROPERTY_DEFINITION('material property','material name',#24234);
#13471=PROPERTY_DEFINITION('material property','density of part',#24234);
#13472=PROPERTY_DEFINITION('material property','material name',#24235);
#13473=PROPERTY_DEFINITION('material property','density of part',#24235);
#13474=PROPERTY_DEFINITION('material property','material name',#24236);
#13475=PROPERTY_DEFINITION('material property','density of part',#24236);
#13476=PROPERTY_DEFINITION('material property','material name',#24237);
#13477=PROPERTY_DEFINITION('material property','density of part',#24237);
#13478=PROPERTY_DEFINITION('material property','material name',#24238);
#13479=PROPERTY_DEFINITION('material property','density of part',#24238);
#13480=PROPERTY_DEFINITION('material property','material name',#24239);
#13481=PROPERTY_DEFINITION('material property','density of part',#24239);
#13482=PROPERTY_DEFINITION('material property','material name',#24240);
#13483=PROPERTY_DEFINITION('material property','density of part',#24240);
#13484=PROPERTY_DEFINITION('material property','material name',#24241);
#13485=PROPERTY_DEFINITION('material property','density of part',#24241);
#13486=PROPERTY_DEFINITION('material property','material name',#24242);
#13487=PROPERTY_DEFINITION('material property','density of part',#24242);
#13488=PROPERTY_DEFINITION('material property','material name',#24243);
#13489=PROPERTY_DEFINITION('material property','density of part',#24243);
#13490=PROPERTY_DEFINITION('material property','material name',#24244);
#13491=PROPERTY_DEFINITION('material property','density of part',#24244);
#13492=PROPERTY_DEFINITION('material property','material name',#24245);
#13493=PROPERTY_DEFINITION('material property','density of part',#24245);
#13494=PROPERTY_DEFINITION('material property','material name',#24246);
#13495=PROPERTY_DEFINITION('material property','density of part',#24246);
#13496=PROPERTY_DEFINITION('material property','material name',#24247);
#13497=PROPERTY_DEFINITION('material property','density of part',#24247);
#13498=PROPERTY_DEFINITION('material property','material name',#24248);
#13499=PROPERTY_DEFINITION('material property','density of part',#24248);
#13500=PROPERTY_DEFINITION('material property','material name',#24249);
#13501=PROPERTY_DEFINITION('material property','density of part',#24249);
#13502=PROPERTY_DEFINITION('material property','material name',#24250);
#13503=PROPERTY_DEFINITION('material property','density of part',#24250);
#13504=PROPERTY_DEFINITION('material property','material name',#24251);
#13505=PROPERTY_DEFINITION('material property','density of part',#24251);
#13506=PROPERTY_DEFINITION('material property','material name',#24252);
#13507=PROPERTY_DEFINITION('material property','density of part',#24252);
#13508=PROPERTY_DEFINITION('material property','material name',#24253);
#13509=PROPERTY_DEFINITION('material property','density of part',#24253);
#13510=PROPERTY_DEFINITION('material property','material name',#24254);
#13511=PROPERTY_DEFINITION('material property','density of part',#24254);
#13512=PROPERTY_DEFINITION('material property','material name',#24255);
#13513=PROPERTY_DEFINITION('material property','density of part',#24255);
#13514=PROPERTY_DEFINITION('material property','material name',#24256);
#13515=PROPERTY_DEFINITION('material property','density of part',#24256);
#13516=PROPERTY_DEFINITION('material property','material name',#24257);
#13517=PROPERTY_DEFINITION('material property','density of part',#24257);
#13518=PROPERTY_DEFINITION('material property','material name',#24258);
#13519=PROPERTY_DEFINITION('material property','density of part',#24258);
#13520=PROPERTY_DEFINITION('material property','material name',#24259);
#13521=PROPERTY_DEFINITION('material property','density of part',#24259);
#13522=PROPERTY_DEFINITION('material property','material name',#24260);
#13523=PROPERTY_DEFINITION('material property','density of part',#24260);
#13524=PROPERTY_DEFINITION('material property','material name',#24262);
#13525=PROPERTY_DEFINITION('material property','density of part',#24262);
#13526=PROPERTY_DEFINITION('material property','material name',#24263);
#13527=PROPERTY_DEFINITION('material property','density of part',#24263);
#13528=PROPERTY_DEFINITION('material property','material name',#24264);
#13529=PROPERTY_DEFINITION('material property','density of part',#24264);
#13530=PROPERTY_DEFINITION('material property','material name',#24265);
#13531=PROPERTY_DEFINITION('material property','density of part',#24265);
#13532=PROPERTY_DEFINITION('material property','material name',#24266);
#13533=PROPERTY_DEFINITION('material property','density of part',#24266);
#13534=PROPERTY_DEFINITION('material property','material name',#24267);
#13535=PROPERTY_DEFINITION('material property','density of part',#24267);
#13536=PROPERTY_DEFINITION('material property','material name',#24268);
#13537=PROPERTY_DEFINITION('material property','density of part',#24268);
#13538=PROPERTY_DEFINITION('material property','material name',#24269);
#13539=PROPERTY_DEFINITION('material property','density of part',#24269);
#13540=PROPERTY_DEFINITION('material property','material name',#24270);
#13541=PROPERTY_DEFINITION('material property','density of part',#24270);
#13542=PROPERTY_DEFINITION('material property','material name',#24271);
#13543=PROPERTY_DEFINITION('material property','density of part',#24271);
#13544=PROPERTY_DEFINITION('material property','material name',#24272);
#13545=PROPERTY_DEFINITION('material property','density of part',#24272);
#13546=PROPERTY_DEFINITION('material property','material name',#24273);
#13547=PROPERTY_DEFINITION('material property','density of part',#24273);
#13548=PROPERTY_DEFINITION('material property','material name',#24274);
#13549=PROPERTY_DEFINITION('material property','density of part',#24274);
#13550=PROPERTY_DEFINITION('material property','material name',#24275);
#13551=PROPERTY_DEFINITION('material property','density of part',#24275);
#13552=PROPERTY_DEFINITION('material property','material name',#24276);
#13553=PROPERTY_DEFINITION('material property','density of part',#24276);
#13554=PROPERTY_DEFINITION('material property','material name',#24277);
#13555=PROPERTY_DEFINITION('material property','density of part',#24277);
#13556=PROPERTY_DEFINITION('material property','material name',#24278);
#13557=PROPERTY_DEFINITION('material property','density of part',#24278);
#13558=PROPERTY_DEFINITION('material property','material name',#24279);
#13559=PROPERTY_DEFINITION('material property','density of part',#24279);
#13560=PROPERTY_DEFINITION('material property','material name',#24280);
#13561=PROPERTY_DEFINITION('material property','density of part',#24280);
#13562=PROPERTY_DEFINITION('material property','material name',#24281);
#13563=PROPERTY_DEFINITION('material property','density of part',#24281);
#13564=PROPERTY_DEFINITION('material property','material name',#24282);
#13565=PROPERTY_DEFINITION('material property','density of part',#24282);
#13566=PROPERTY_DEFINITION('material property','material name',#24284);
#13567=PROPERTY_DEFINITION('material property','density of part',#24284);
#13568=PROPERTY_DEFINITION('material property','material name',#24285);
#13569=PROPERTY_DEFINITION('material property','density of part',#24285);
#13570=PROPERTY_DEFINITION('material property','material name',#24286);
#13571=PROPERTY_DEFINITION('material property','density of part',#24286);
#13572=PROPERTY_DEFINITION('material property','material name',#24287);
#13573=PROPERTY_DEFINITION('material property','density of part',#24287);
#13574=PROPERTY_DEFINITION('material property','material name',#24288);
#13575=PROPERTY_DEFINITION('material property','density of part',#24288);
#13576=PROPERTY_DEFINITION('material property','material name',#24289);
#13577=PROPERTY_DEFINITION('material property','density of part',#24289);
#13578=PROPERTY_DEFINITION('material property','material name',#24290);
#13579=PROPERTY_DEFINITION('material property','density of part',#24290);
#13580=PROPERTY_DEFINITION('material property','material name',#24291);
#13581=PROPERTY_DEFINITION('material property','density of part',#24291);
#13582=PROPERTY_DEFINITION('material property','material name',#24292);
#13583=PROPERTY_DEFINITION('material property','density of part',#24292);
#13584=PROPERTY_DEFINITION('material property','material name',#24293);
#13585=PROPERTY_DEFINITION('material property','density of part',#24293);
#13586=PROPERTY_DEFINITION('material property','material name',#24294);
#13587=PROPERTY_DEFINITION('material property','density of part',#24294);
#13588=PROPERTY_DEFINITION('material property','material name',#24295);
#13589=PROPERTY_DEFINITION('material property','density of part',#24295);
#13590=PROPERTY_DEFINITION('material property','material name',#24296);
#13591=PROPERTY_DEFINITION('material property','density of part',#24296);
#13592=PROPERTY_DEFINITION('material property','material name',#24297);
#13593=PROPERTY_DEFINITION('material property','density of part',#24297);
#13594=PROPERTY_DEFINITION('material property','material name',#24298);
#13595=PROPERTY_DEFINITION('material property','density of part',#24298);
#13596=PROPERTY_DEFINITION('material property','material name',#24299);
#13597=PROPERTY_DEFINITION('material property','density of part',#24299);
#13598=PROPERTY_DEFINITION('material property','material name',#24300);
#13599=PROPERTY_DEFINITION('material property','density of part',#24300);
#13600=PROPERTY_DEFINITION('material property','material name',#24301);
#13601=PROPERTY_DEFINITION('material property','density of part',#24301);
#13602=PROPERTY_DEFINITION('material property','material name',#24302);
#13603=PROPERTY_DEFINITION('material property','density of part',#24302);
#13604=PROPERTY_DEFINITION('material property','material name',#24303);
#13605=PROPERTY_DEFINITION('material property','density of part',#24303);
#13606=PROPERTY_DEFINITION('material property','material name',#24304);
#13607=PROPERTY_DEFINITION('material property','density of part',#24304);
#13608=PROPERTY_DEFINITION('material property','material name',#24306);
#13609=PROPERTY_DEFINITION('material property','density of part',#24306);
#13610=PROPERTY_DEFINITION('material property','material name',#24307);
#13611=PROPERTY_DEFINITION('material property','density of part',#24307);
#13612=PROPERTY_DEFINITION('material property','material name',#24308);
#13613=PROPERTY_DEFINITION('material property','density of part',#24308);
#13614=PROPERTY_DEFINITION('material property','material name',#24309);
#13615=PROPERTY_DEFINITION('material property','density of part',#24309);
#13616=PROPERTY_DEFINITION('material property','material name',#24310);
#13617=PROPERTY_DEFINITION('material property','density of part',#24310);
#13618=PROPERTY_DEFINITION('material property','material name',#24312);
#13619=PROPERTY_DEFINITION('material property','density of part',#24312);
#13620=PROPERTY_DEFINITION('material property','material name',#24313);
#13621=PROPERTY_DEFINITION('material property','density of part',#24313);
#13622=PROPERTY_DEFINITION('material property','material name',#24314);
#13623=PROPERTY_DEFINITION('material property','density of part',#24314);
#13624=PROPERTY_DEFINITION('material property','material name',#24315);
#13625=PROPERTY_DEFINITION('material property','density of part',#24315);
#13626=PROPERTY_DEFINITION('material property','material name',#24316);
#13627=PROPERTY_DEFINITION('material property','density of part',#24316);
#13628=PROPERTY_DEFINITION('material property','material name',#24317);
#13629=PROPERTY_DEFINITION('material property','density of part',#24317);
#13630=PROPERTY_DEFINITION('material property','material name',#24318);
#13631=PROPERTY_DEFINITION('material property','density of part',#24318);
#13632=PROPERTY_DEFINITION('material property','material name',#24319);
#13633=PROPERTY_DEFINITION('material property','density of part',#24319);
#13634=PROPERTY_DEFINITION('material property','material name',#24320);
#13635=PROPERTY_DEFINITION('material property','density of part',#24320);
#13636=PROPERTY_DEFINITION('material property','material name',#24321);
#13637=PROPERTY_DEFINITION('material property','density of part',#24321);
#13638=PROPERTY_DEFINITION('material property','material name',#24322);
#13639=PROPERTY_DEFINITION('material property','density of part',#24322);
#13640=PROPERTY_DEFINITION('material property','material name',#24323);
#13641=PROPERTY_DEFINITION('material property','density of part',#24323);
#13642=PROPERTY_DEFINITION('material property','material name',#24324);
#13643=PROPERTY_DEFINITION('material property','density of part',#24324);
#13644=PROPERTY_DEFINITION('material property','material name',#24326);
#13645=PROPERTY_DEFINITION('material property','density of part',#24326);
#13646=PROPERTY_DEFINITION('material property','material name',#24327);
#13647=PROPERTY_DEFINITION('material property','density of part',#24327);
#13648=PROPERTY_DEFINITION('material property','material name',#24328);
#13649=PROPERTY_DEFINITION('material property','density of part',#24328);
#13650=PROPERTY_DEFINITION('material property','material name',#24329);
#13651=PROPERTY_DEFINITION('material property','density of part',#24329);
#13652=PROPERTY_DEFINITION('material property','material name',#24330);
#13653=PROPERTY_DEFINITION('material property','density of part',#24330);
#13654=PROPERTY_DEFINITION('material property','material name',#24331);
#13655=PROPERTY_DEFINITION('material property','density of part',#24331);
#13656=PROPERTY_DEFINITION('material property','material name',#24332);
#13657=PROPERTY_DEFINITION('material property','density of part',#24332);
#13658=PROPERTY_DEFINITION('material property','material name',#24334);
#13659=PROPERTY_DEFINITION('material property','density of part',#24334);
#13660=PROPERTY_DEFINITION('material property','material name',#24335);
#13661=PROPERTY_DEFINITION('material property','density of part',#24335);
#13662=PROPERTY_DEFINITION('material property','material name',#24336);
#13663=PROPERTY_DEFINITION('material property','density of part',#24336);
#13664=PROPERTY_DEFINITION('material property','material name',#24338);
#13665=PROPERTY_DEFINITION('material property','density of part',#24338);
#13666=PROPERTY_DEFINITION('material property','material name',#24340);
#13667=PROPERTY_DEFINITION('material property','density of part',#24340);
#13668=PROPERTY_DEFINITION('material property','material name',#24341);
#13669=PROPERTY_DEFINITION('material property','density of part',#24341);
#13670=PROPERTY_DEFINITION('material property','material name',#24342);
#13671=PROPERTY_DEFINITION('material property','density of part',#24342);
#13672=PROPERTY_DEFINITION('material property','material name',#24343);
#13673=PROPERTY_DEFINITION('material property','density of part',#24343);
#13674=PROPERTY_DEFINITION('material property','material name',#24344);
#13675=PROPERTY_DEFINITION('material property','density of part',#24344);
#13676=AXIS2_PLACEMENT_3D('',#19745,#15474,#15475);
#13677=AXIS2_PLACEMENT_3D('',#19746,#15476,#15477);
#13678=AXIS2_PLACEMENT_3D('',#19747,#15478,#15479);
#13679=AXIS2_PLACEMENT_3D('',#19748,#15480,#15481);
#13680=AXIS2_PLACEMENT_3D('',#19750,#15482,#15483);
#13681=AXIS2_PLACEMENT_3D('',#19753,#15485,#15486);
#13682=AXIS2_PLACEMENT_3D('',#19754,#15487,#15488);
#13683=AXIS2_PLACEMENT_3D('',#19756,#15489,#15490);
#13684=AXIS2_PLACEMENT_3D('',#19759,#15492,#15493);
#13685=AXIS2_PLACEMENT_3D('',#19760,#15494,#15495);
#13686=AXIS2_PLACEMENT_3D('',#19762,#15496,#15497);
#13687=AXIS2_PLACEMENT_3D('',#19765,#15499,#15500);
#13688=AXIS2_PLACEMENT_3D('',#19766,#15501,#15502);
#13689=AXIS2_PLACEMENT_3D('',#19768,#15503,#15504);
#13690=AXIS2_PLACEMENT_3D('',#19771,#15506,#15507);
#13691=AXIS2_PLACEMENT_3D('',#19772,#15508,#15509);
#13692=AXIS2_PLACEMENT_3D('',#19774,#15510,#15511);
#13693=AXIS2_PLACEMENT_3D('',#19777,#15513,#15514);
#13694=AXIS2_PLACEMENT_3D('',#19778,#15515,#15516);
#13695=AXIS2_PLACEMENT_3D('',#19780,#15517,#15518);
#13696=AXIS2_PLACEMENT_3D('',#19783,#15520,#15521);
#13697=AXIS2_PLACEMENT_3D('',#19784,#15522,#15523);
#13698=AXIS2_PLACEMENT_3D('',#19786,#15524,#15525);
#13699=AXIS2_PLACEMENT_3D('',#19789,#15527,#15528);
#13700=AXIS2_PLACEMENT_3D('',#19790,#15529,#15530);
#13701=AXIS2_PLACEMENT_3D('',#19792,#15531,#15532);
#13702=AXIS2_PLACEMENT_3D('',#19795,#15534,#15535);
#13703=AXIS2_PLACEMENT_3D('',#19796,#15536,#15537);
#13704=AXIS2_PLACEMENT_3D('',#19798,#15538,#15539);
#13705=AXIS2_PLACEMENT_3D('',#19801,#15541,#15542);
#13706=AXIS2_PLACEMENT_3D('',#19802,#15543,#15544);
#13707=AXIS2_PLACEMENT_3D('',#19804,#15545,#15546);
#13708=AXIS2_PLACEMENT_3D('',#19807,#15548,#15549);
#13709=AXIS2_PLACEMENT_3D('',#19808,#15550,#15551);
#13710=AXIS2_PLACEMENT_3D('',#19810,#15552,#15553);
#13711=AXIS2_PLACEMENT_3D('',#19813,#15555,#15556);
#13712=AXIS2_PLACEMENT_3D('',#19814,#15557,#15558);
#13713=AXIS2_PLACEMENT_3D('',#19816,#15559,#15560);
#13714=AXIS2_PLACEMENT_3D('',#19819,#15562,#15563);
#13715=AXIS2_PLACEMENT_3D('',#19820,#15564,#15565);
#13716=AXIS2_PLACEMENT_3D('',#19829,#15570,#15571);
#13717=AXIS2_PLACEMENT_3D('',#19835,#15575,#15576);
#13718=AXIS2_PLACEMENT_3D('',#19841,#15580,#15581);
#13719=AXIS2_PLACEMENT_3D('',#19844,#15584,#15585);
#13720=AXIS2_PLACEMENT_3D('',#19845,#15586,#15587);
#13721=AXIS2_PLACEMENT_3D('',#19846,#15588,#15589);
#13722=AXIS2_PLACEMENT_3D('',#19847,#15590,#15591);
#13723=AXIS2_PLACEMENT_3D('',#19856,#15596,#15597);
#13724=AXIS2_PLACEMENT_3D('',#19862,#15601,#15602);
#13725=AXIS2_PLACEMENT_3D('',#19868,#15606,#15607);
#13726=AXIS2_PLACEMENT_3D('',#19871,#15610,#15611);
#13727=AXIS2_PLACEMENT_3D('',#19872,#15612,#15613);
#13728=AXIS2_PLACEMENT_3D('',#19873,#15614,#15615);
#13729=AXIS2_PLACEMENT_3D('',#19874,#15616,#15617);
#13730=AXIS2_PLACEMENT_3D('',#19883,#15622,#15623);
#13731=AXIS2_PLACEMENT_3D('',#19889,#15627,#15628);
#13732=AXIS2_PLACEMENT_3D('',#19895,#15632,#15633);
#13733=AXIS2_PLACEMENT_3D('',#19898,#15636,#15637);
#13734=AXIS2_PLACEMENT_3D('',#19899,#15638,#15639);
#13735=AXIS2_PLACEMENT_3D('',#19900,#15640,#15641);
#13736=AXIS2_PLACEMENT_3D('',#19901,#15642,#15643);
#13737=AXIS2_PLACEMENT_3D('',#19903,#15644,#15645);
#13738=AXIS2_PLACEMENT_3D('',#19906,#15647,#15648);
#13739=AXIS2_PLACEMENT_3D('',#19907,#15649,#15650);
#13740=AXIS2_PLACEMENT_3D('',#19909,#15651,#15652);
#13741=AXIS2_PLACEMENT_3D('',#19912,#15654,#15655);
#13742=AXIS2_PLACEMENT_3D('',#19913,#15656,#15657);
#13743=AXIS2_PLACEMENT_3D('',#19915,#15658,#15659);
#13744=AXIS2_PLACEMENT_3D('',#19918,#15661,#15662);
#13745=AXIS2_PLACEMENT_3D('',#19919,#15663,#15664);
#13746=AXIS2_PLACEMENT_3D('',#19921,#15665,#15666);
#13747=AXIS2_PLACEMENT_3D('',#19924,#15668,#15669);
#13748=AXIS2_PLACEMENT_3D('',#19925,#15670,#15671);
#13749=AXIS2_PLACEMENT_3D('',#19927,#15672,#15673);
#13750=AXIS2_PLACEMENT_3D('',#19930,#15675,#15676);
#13751=AXIS2_PLACEMENT_3D('',#19931,#15677,#15678);
#13752=AXIS2_PLACEMENT_3D('',#19933,#15679,#15680);
#13753=AXIS2_PLACEMENT_3D('',#19936,#15682,#15683);
#13754=AXIS2_PLACEMENT_3D('',#19937,#15684,#15685);
#13755=AXIS2_PLACEMENT_3D('',#19939,#15686,#15687);
#13756=AXIS2_PLACEMENT_3D('',#19942,#15689,#15690);
#13757=AXIS2_PLACEMENT_3D('',#19943,#15691,#15692);
#13758=AXIS2_PLACEMENT_3D('',#19945,#15693,#15694);
#13759=AXIS2_PLACEMENT_3D('',#19948,#15696,#15697);
#13760=AXIS2_PLACEMENT_3D('',#19949,#15698,#15699);
#13761=AXIS2_PLACEMENT_3D('',#19966,#15708,#15709);
#13762=AXIS2_PLACEMENT_3D('',#19972,#15713,#15714);
#13763=AXIS2_PLACEMENT_3D('',#19978,#15718,#15719);
#13764=AXIS2_PLACEMENT_3D('',#19980,#15721,#15722);
#13765=AXIS2_PLACEMENT_3D('',#19987,#15727,#15728);
#13766=AXIS2_PLACEMENT_3D('',#19991,#15731,#15732);
#13767=AXIS2_PLACEMENT_3D('',#19995,#15735,#15736);
#13768=AXIS2_PLACEMENT_3D('',#19997,#15738,#15739);
#13769=AXIS2_PLACEMENT_3D('',#19998,#15740,#15741);
#13770=AXIS2_PLACEMENT_3D('',#19999,#15742,#15743);
#13771=AXIS2_PLACEMENT_3D('',#20000,#15744,#15745);
#13772=AXIS2_PLACEMENT_3D('',#20002,#15746,#15747);
#13773=AXIS2_PLACEMENT_3D('',#20005,#15749,#15750);
#13774=AXIS2_PLACEMENT_3D('',#20006,#15751,#15752);
#13775=AXIS2_PLACEMENT_3D('',#20008,#15753,#15754);
#13776=AXIS2_PLACEMENT_3D('',#20011,#15756,#15757);
#13777=AXIS2_PLACEMENT_3D('',#20012,#15758,#15759);
#13778=AXIS2_PLACEMENT_3D('',#20014,#15760,#15761);
#13779=AXIS2_PLACEMENT_3D('',#20017,#15763,#15764);
#13780=AXIS2_PLACEMENT_3D('',#20018,#15765,#15766);
#13781=AXIS2_PLACEMENT_3D('',#20020,#15767,#15768);
#13782=AXIS2_PLACEMENT_3D('',#20023,#15770,#15771);
#13783=AXIS2_PLACEMENT_3D('',#20024,#15772,#15773);
#13784=AXIS2_PLACEMENT_3D('',#20026,#15774,#15775);
#13785=AXIS2_PLACEMENT_3D('',#20029,#15777,#15778);
#13786=AXIS2_PLACEMENT_3D('',#20030,#15779,#15780);
#13787=AXIS2_PLACEMENT_3D('',#20032,#15781,#15782);
#13788=AXIS2_PLACEMENT_3D('',#20035,#15784,#15785);
#13789=AXIS2_PLACEMENT_3D('',#20036,#15786,#15787);
#13790=AXIS2_PLACEMENT_3D('',#20038,#15788,#15789);
#13791=AXIS2_PLACEMENT_3D('',#20041,#15791,#15792);
#13792=AXIS2_PLACEMENT_3D('',#20042,#15793,#15794);
#13793=AXIS2_PLACEMENT_3D('',#20044,#15795,#15796);
#13794=AXIS2_PLACEMENT_3D('',#20047,#15798,#15799);
#13795=AXIS2_PLACEMENT_3D('',#20048,#15800,#15801);
#13796=AXIS2_PLACEMENT_3D('',#20065,#15810,#15811);
#13797=AXIS2_PLACEMENT_3D('',#20071,#15815,#15816);
#13798=AXIS2_PLACEMENT_3D('',#20077,#15820,#15821);
#13799=AXIS2_PLACEMENT_3D('',#20079,#15823,#15824);
#13800=AXIS2_PLACEMENT_3D('',#20086,#15829,#15830);
#13801=AXIS2_PLACEMENT_3D('',#20090,#15833,#15834);
#13802=AXIS2_PLACEMENT_3D('',#20094,#15837,#15838);
#13803=AXIS2_PLACEMENT_3D('',#20096,#15840,#15841);
#13804=AXIS2_PLACEMENT_3D('',#20097,#15842,#15843);
#13805=AXIS2_PLACEMENT_3D('',#20098,#15844,#15845);
#13806=AXIS2_PLACEMENT_3D('',#20099,#15846,#15847);
#13807=AXIS2_PLACEMENT_3D('',#20101,#15848,#15849);
#13808=AXIS2_PLACEMENT_3D('',#20104,#15851,#15852);
#13809=AXIS2_PLACEMENT_3D('',#20105,#15853,#15854);
#13810=AXIS2_PLACEMENT_3D('',#20106,#15855,#15856);
#13811=AXIS2_PLACEMENT_3D('',#20108,#15857,#15858);
#13812=AXIS2_PLACEMENT_3D('',#20111,#15860,#15861);
#13813=AXIS2_PLACEMENT_3D('',#20112,#15862,#15863);
#13814=AXIS2_PLACEMENT_3D('',#20114,#15864,#15865);
#13815=AXIS2_PLACEMENT_3D('',#20117,#15867,#15868);
#13816=AXIS2_PLACEMENT_3D('',#20118,#15869,#15870);
#13817=AXIS2_PLACEMENT_3D('',#20120,#15871,#15872);
#13818=AXIS2_PLACEMENT_3D('',#20123,#15874,#15875);
#13819=AXIS2_PLACEMENT_3D('',#20124,#15876,#15877);
#13820=AXIS2_PLACEMENT_3D('',#20126,#15878,#15879);
#13821=AXIS2_PLACEMENT_3D('',#20128,#15880,#15881);
#13822=AXIS2_PLACEMENT_3D('',#20129,#15882,#15883);
#13823=AXIS2_PLACEMENT_3D('',#20131,#15884,#15885);
#13824=AXIS2_PLACEMENT_3D('',#20133,#15886,#15887);
#13825=AXIS2_PLACEMENT_3D('',#20134,#15888,#15889);
#13826=AXIS2_PLACEMENT_3D('',#20136,#15891,#15892);
#13827=AXIS2_PLACEMENT_3D('',#20139,#15894,#15895);
#13828=AXIS2_PLACEMENT_3D('',#20140,#15896,#15897);
#13829=AXIS2_PLACEMENT_3D('',#20142,#15898,#15899);
#13830=AXIS2_PLACEMENT_3D('',#20144,#15901,#15902);
#13831=AXIS2_PLACEMENT_3D('',#20145,#15903,#15904);
#13832=AXIS2_PLACEMENT_3D('',#20146,#15905,#15906);
#13833=AXIS2_PLACEMENT_3D('',#20147,#15907,#15908);
#13834=AXIS2_PLACEMENT_3D('',#20149,#15909,#15910);
#13835=AXIS2_PLACEMENT_3D('',#20152,#15912,#15913);
#13836=AXIS2_PLACEMENT_3D('',#20153,#15914,#15915);
#13837=AXIS2_PLACEMENT_3D('',#20155,#15916,#15917);
#13838=AXIS2_PLACEMENT_3D('',#20158,#15919,#15920);
#13839=AXIS2_PLACEMENT_3D('',#20159,#15921,#15922);
#13840=AXIS2_PLACEMENT_3D('',#20160,#15923,#15924);
#13841=AXIS2_PLACEMENT_3D('',#20161,#15925,#15926);
#13842=AXIS2_PLACEMENT_3D('',#20162,#15927,#15928);
#13843=AXIS2_PLACEMENT_3D('',#20164,#15929,#15930);
#13844=AXIS2_PLACEMENT_3D('',#20167,#15932,#15933);
#13845=AXIS2_PLACEMENT_3D('',#20168,#15934,#15935);
#13846=AXIS2_PLACEMENT_3D('',#20170,#15936,#15937);
#13847=AXIS2_PLACEMENT_3D('',#20173,#15939,#15940);
#13848=AXIS2_PLACEMENT_3D('',#20174,#15941,#15942);
#13849=AXIS2_PLACEMENT_3D('',#20175,#15943,#15944);
#13850=AXIS2_PLACEMENT_3D('',#20176,#15945,#15946);
#13851=AXIS2_PLACEMENT_3D('',#20177,#15947,#15948);
#13852=AXIS2_PLACEMENT_3D('',#20179,#15949,#15950);
#13853=AXIS2_PLACEMENT_3D('',#20182,#15952,#15953);
#13854=AXIS2_PLACEMENT_3D('',#20183,#15954,#15955);
#13855=AXIS2_PLACEMENT_3D('',#20185,#15956,#15957);
#13856=AXIS2_PLACEMENT_3D('',#20188,#15959,#15960);
#13857=AXIS2_PLACEMENT_3D('',#20189,#15961,#15962);
#13858=AXIS2_PLACEMENT_3D('',#20190,#15963,#15964);
#13859=AXIS2_PLACEMENT_3D('',#20191,#15965,#15966);
#13860=AXIS2_PLACEMENT_3D('',#20192,#15967,#15968);
#13861=AXIS2_PLACEMENT_3D('',#20194,#15969,#15970);
#13862=AXIS2_PLACEMENT_3D('',#20197,#15972,#15973);
#13863=AXIS2_PLACEMENT_3D('',#20198,#15974,#15975);
#13864=AXIS2_PLACEMENT_3D('',#20199,#15976,#15977);
#13865=AXIS2_PLACEMENT_3D('',#20201,#15978,#15979);
#13866=AXIS2_PLACEMENT_3D('',#20204,#15981,#15982);
#13867=AXIS2_PLACEMENT_3D('',#20205,#15983,#15984);
#13868=AXIS2_PLACEMENT_3D('',#20207,#15985,#15986);
#13869=AXIS2_PLACEMENT_3D('',#20210,#15988,#15989);
#13870=AXIS2_PLACEMENT_3D('',#20211,#15990,#15991);
#13871=AXIS2_PLACEMENT_3D('',#20213,#15992,#15993);
#13872=AXIS2_PLACEMENT_3D('',#20216,#15995,#15996);
#13873=AXIS2_PLACEMENT_3D('',#20217,#15997,#15998);
#13874=AXIS2_PLACEMENT_3D('',#20219,#15999,#16000);
#13875=AXIS2_PLACEMENT_3D('',#20221,#16001,#16002);
#13876=AXIS2_PLACEMENT_3D('',#20222,#16003,#16004);
#13877=AXIS2_PLACEMENT_3D('',#20224,#16005,#16006);
#13878=AXIS2_PLACEMENT_3D('',#20226,#16007,#16008);
#13879=AXIS2_PLACEMENT_3D('',#20227,#16009,#16010);
#13880=AXIS2_PLACEMENT_3D('',#20229,#16012,#16013);
#13881=AXIS2_PLACEMENT_3D('',#20232,#16015,#16016);
#13882=AXIS2_PLACEMENT_3D('',#20233,#16017,#16018);
#13883=AXIS2_PLACEMENT_3D('',#20235,#16019,#16020);
#13884=AXIS2_PLACEMENT_3D('',#20237,#16022,#16023);
#13885=AXIS2_PLACEMENT_3D('',#20238,#16024,#16025);
#13886=AXIS2_PLACEMENT_3D('',#20239,#16026,#16027);
#13887=AXIS2_PLACEMENT_3D('',#20240,#16028,#16029);
#13888=AXIS2_PLACEMENT_3D('',#20242,#16030,#16031);
#13889=AXIS2_PLACEMENT_3D('',#20245,#16033,#16034);
#13890=AXIS2_PLACEMENT_3D('',#20246,#16035,#16036);
#13891=AXIS2_PLACEMENT_3D('',#20248,#16037,#16038);
#13892=AXIS2_PLACEMENT_3D('',#20251,#16040,#16041);
#13893=AXIS2_PLACEMENT_3D('',#20252,#16042,#16043);
#13894=AXIS2_PLACEMENT_3D('',#20253,#16044,#16045);
#13895=AXIS2_PLACEMENT_3D('',#20254,#16046,#16047);
#13896=AXIS2_PLACEMENT_3D('',#20255,#16048,#16049);
#13897=AXIS2_PLACEMENT_3D('',#20257,#16050,#16051);
#13898=AXIS2_PLACEMENT_3D('',#20260,#16053,#16054);
#13899=AXIS2_PLACEMENT_3D('',#20261,#16055,#16056);
#13900=AXIS2_PLACEMENT_3D('',#20263,#16057,#16058);
#13901=AXIS2_PLACEMENT_3D('',#20266,#16060,#16061);
#13902=AXIS2_PLACEMENT_3D('',#20267,#16062,#16063);
#13903=AXIS2_PLACEMENT_3D('',#20268,#16064,#16065);
#13904=AXIS2_PLACEMENT_3D('',#20269,#16066,#16067);
#13905=AXIS2_PLACEMENT_3D('',#20270,#16068,#16069);
#13906=AXIS2_PLACEMENT_3D('',#20272,#16070,#16071);
#13907=AXIS2_PLACEMENT_3D('',#20275,#16073,#16074);
#13908=AXIS2_PLACEMENT_3D('',#20276,#16075,#16076);
#13909=AXIS2_PLACEMENT_3D('',#20278,#16077,#16078);
#13910=AXIS2_PLACEMENT_3D('',#20281,#16080,#16081);
#13911=AXIS2_PLACEMENT_3D('',#20282,#16082,#16083);
#13912=AXIS2_PLACEMENT_3D('',#20283,#16084,#16085);
#13913=AXIS2_PLACEMENT_3D('',#20284,#16086,#16087);
#13914=AXIS2_PLACEMENT_3D('',#20285,#16088,#16089);
#13915=AXIS2_PLACEMENT_3D('',#20288,#16090,#16091);
#13916=AXIS2_PLACEMENT_3D('',#20292,#16093,#16094);
#13917=AXIS2_PLACEMENT_3D('',#20294,#16096,#16097);
#13918=AXIS2_PLACEMENT_3D('',#20296,#16098,#16099);
#13919=AXIS2_PLACEMENT_3D('',#20299,#16101,#16102);
#13920=AXIS2_PLACEMENT_3D('',#20300,#16103,#16104);
#13921=AXIS2_PLACEMENT_3D('',#20307,#16108,#16109);
#13922=AXIS2_PLACEMENT_3D('',#20308,#16110,#16111);
#13923=AXIS2_PLACEMENT_3D('',#20317,#16116,#16117);
#13924=AXIS2_PLACEMENT_3D('',#20319,#16118,#16119);
#13925=AXIS2_PLACEMENT_3D('',#20321,#16120,#16121);
#13926=AXIS2_PLACEMENT_3D('',#20322,#16122,#16123);
#13927=AXIS2_PLACEMENT_3D('',#20324,#16124,#16125);
#13928=AXIS2_PLACEMENT_3D('',#20327,#16127,#16128);
#13929=AXIS2_PLACEMENT_3D('',#20328,#16129,#16130);
#13930=AXIS2_PLACEMENT_3D('',#20330,#16131,#16132);
#13931=AXIS2_PLACEMENT_3D('',#20331,#16133,#16134);
#13932=AXIS2_PLACEMENT_3D('',#20333,#16135,#16136);
#13933=AXIS2_PLACEMENT_3D('',#20335,#16138,#16139);
#13934=AXIS2_PLACEMENT_3D('',#20337,#16140,#16141);
#13935=AXIS2_PLACEMENT_3D('',#20339,#16143,#16144);
#13936=AXIS2_PLACEMENT_3D('',#20341,#16145,#16146);
#13937=AXIS2_PLACEMENT_3D('',#20342,#16147,#16148);
#13938=AXIS2_PLACEMENT_3D('',#20344,#16149,#16150);
#13939=AXIS2_PLACEMENT_3D('',#20346,#16152,#16153);
#13940=AXIS2_PLACEMENT_3D('',#20348,#16154,#16155);
#13941=AXIS2_PLACEMENT_3D('',#20350,#16157,#16158);
#13942=AXIS2_PLACEMENT_3D('',#20352,#16159,#16160);
#13943=AXIS2_PLACEMENT_3D('',#20354,#16162,#16163);
#13944=AXIS2_PLACEMENT_3D('',#20356,#16164,#16165);
#13945=AXIS2_PLACEMENT_3D('',#20358,#16167,#16168);
#13946=AXIS2_PLACEMENT_3D('',#20364,#16172,#16173);
#13947=AXIS2_PLACEMENT_3D('',#20368,#16176,#16177);
#13948=AXIS2_PLACEMENT_3D('',#20371,#16180,#16181);
#13949=AXIS2_PLACEMENT_3D('',#20372,#16182,#16183);
#13950=AXIS2_PLACEMENT_3D('',#20373,#16184,#16185);
#13951=AXIS2_PLACEMENT_3D('',#20374,#16186,#16187);
#13952=AXIS2_PLACEMENT_3D('',#20376,#16188,#16189);
#13953=AXIS2_PLACEMENT_3D('',#20379,#16191,#16192);
#13954=AXIS2_PLACEMENT_3D('',#20380,#16193,#16194);
#13955=AXIS2_PLACEMENT_3D('',#20382,#16195,#16196);
#13956=AXIS2_PLACEMENT_3D('',#20385,#16198,#16199);
#13957=AXIS2_PLACEMENT_3D('',#20386,#16200,#16201);
#13958=AXIS2_PLACEMENT_3D('',#20391,#16203,#16204);
#13959=AXIS2_PLACEMENT_3D('',#20394,#16206,#16207);
#13960=AXIS2_PLACEMENT_3D('',#20395,#16208,#16209);
#13961=AXIS2_PLACEMENT_3D('',#20400,#16211,#16212);
#13962=AXIS2_PLACEMENT_3D('',#20403,#16214,#16215);
#13963=AXIS2_PLACEMENT_3D('',#20404,#16216,#16217);
#13964=AXIS2_PLACEMENT_3D('',#20405,#16218,#16219);
#13965=AXIS2_PLACEMENT_3D('',#20406,#16220,#16221);
#13966=AXIS2_PLACEMENT_3D('',#20408,#16222,#16223);
#13967=AXIS2_PLACEMENT_3D('',#20409,#16224,#16225);
#13968=AXIS2_PLACEMENT_3D('',#20410,#16226,#16227);
#13969=AXIS2_PLACEMENT_3D('',#20411,#16228,#16229);
#13970=AXIS2_PLACEMENT_3D('',#20412,#16230,#16231);
#13971=AXIS2_PLACEMENT_3D('',#20413,#16232,#16233);
#13972=AXIS2_PLACEMENT_3D('',#20416,#16235,#16236);
#13973=AXIS2_PLACEMENT_3D('',#20417,#16237,#16238);
#13974=AXIS2_PLACEMENT_3D('',#20418,#16239,#16240);
#13975=AXIS2_PLACEMENT_3D('',#20419,#16241,#16242);
#13976=AXIS2_PLACEMENT_3D('',#20421,#16243,#16244);
#13977=AXIS2_PLACEMENT_3D('',#20423,#16245,#16246);
#13978=AXIS2_PLACEMENT_3D('',#20424,#16247,#16248);
#13979=AXIS2_PLACEMENT_3D('',#20427,#16250,#16251);
#13980=AXIS2_PLACEMENT_3D('',#20428,#16252,#16253);
#13981=AXIS2_PLACEMENT_3D('',#20429,#16254,#16255);
#13982=AXIS2_PLACEMENT_3D('',#20431,#16256,#16257);
#13983=AXIS2_PLACEMENT_3D('',#20433,#16259,#16260);
#13984=AXIS2_PLACEMENT_3D('',#20434,#16261,#16262);
#13985=AXIS2_PLACEMENT_3D('',#20435,#16263,#16264);
#13986=AXIS2_PLACEMENT_3D('',#20437,#16265,#16266);
#13987=AXIS2_PLACEMENT_3D('',#20439,#16267,#16268);
#13988=AXIS2_PLACEMENT_3D('',#20440,#16269,#16270);
#13989=AXIS2_PLACEMENT_3D('',#20443,#16272,#16273);
#13990=AXIS2_PLACEMENT_3D('',#20444,#16274,#16275);
#13991=AXIS2_PLACEMENT_3D('',#20445,#16276,#16277);
#13992=AXIS2_PLACEMENT_3D('',#20447,#16278,#16279);
#13993=AXIS2_PLACEMENT_3D('',#20449,#16281,#16282);
#13994=AXIS2_PLACEMENT_3D('',#20450,#16283,#16284);
#13995=AXIS2_PLACEMENT_3D('',#20451,#16285,#16286);
#13996=AXIS2_PLACEMENT_3D('',#20453,#16287,#16288);
#13997=AXIS2_PLACEMENT_3D('',#20456,#16290,#16291);
#13998=AXIS2_PLACEMENT_3D('',#20457,#16292,#16293);
#13999=AXIS2_PLACEMENT_3D('',#20459,#16294,#16295);
#14000=AXIS2_PLACEMENT_3D('',#20462,#16297,#16298);
#14001=AXIS2_PLACEMENT_3D('',#20463,#16299,#16300);
#14002=AXIS2_PLACEMENT_3D('',#20468,#16302,#16303);
#14003=AXIS2_PLACEMENT_3D('',#20471,#16305,#16306);
#14004=AXIS2_PLACEMENT_3D('',#20472,#16307,#16308);
#14005=AXIS2_PLACEMENT_3D('',#20477,#16310,#16311);
#14006=AXIS2_PLACEMENT_3D('',#20480,#16313,#16314);
#14007=AXIS2_PLACEMENT_3D('',#20481,#16315,#16316);
#14008=AXIS2_PLACEMENT_3D('',#20482,#16317,#16318);
#14009=AXIS2_PLACEMENT_3D('',#20483,#16319,#16320);
#14010=AXIS2_PLACEMENT_3D('',#20485,#16321,#16322);
#14011=AXIS2_PLACEMENT_3D('',#20486,#16323,#16324);
#14012=AXIS2_PLACEMENT_3D('',#20487,#16325,#16326);
#14013=AXIS2_PLACEMENT_3D('',#20488,#16327,#16328);
#14014=AXIS2_PLACEMENT_3D('',#20489,#16329,#16330);
#14015=AXIS2_PLACEMENT_3D('',#20490,#16331,#16332);
#14016=AXIS2_PLACEMENT_3D('',#20493,#16334,#16335);
#14017=AXIS2_PLACEMENT_3D('',#20494,#16336,#16337);
#14018=AXIS2_PLACEMENT_3D('',#20495,#16338,#16339);
#14019=AXIS2_PLACEMENT_3D('',#20496,#16340,#16341);
#14020=AXIS2_PLACEMENT_3D('',#20498,#16342,#16343);
#14021=AXIS2_PLACEMENT_3D('',#20500,#16344,#16345);
#14022=AXIS2_PLACEMENT_3D('',#20501,#16346,#16347);
#14023=AXIS2_PLACEMENT_3D('',#20503,#16348,#16349);
#14024=AXIS2_PLACEMENT_3D('',#20505,#16351,#16352);
#14025=AXIS2_PLACEMENT_3D('',#20506,#16353,#16354);
#14026=AXIS2_PLACEMENT_3D('',#20509,#16356,#16357);
#14027=AXIS2_PLACEMENT_3D('',#20510,#16358,#16359);
#14028=AXIS2_PLACEMENT_3D('',#20511,#16360,#16361);
#14029=AXIS2_PLACEMENT_3D('',#20512,#16362,#16363);
#14030=AXIS2_PLACEMENT_3D('',#20514,#16364,#16365);
#14031=AXIS2_PLACEMENT_3D('',#20516,#16366,#16367);
#14032=AXIS2_PLACEMENT_3D('',#20517,#16368,#16369);
#14033=AXIS2_PLACEMENT_3D('',#20519,#16370,#16371);
#14034=AXIS2_PLACEMENT_3D('',#20521,#16373,#16374);
#14035=AXIS2_PLACEMENT_3D('',#20522,#16375,#16376);
#14036=AXIS2_PLACEMENT_3D('',#20525,#16378,#16379);
#14037=AXIS2_PLACEMENT_3D('',#20526,#16380,#16381);
#14038=AXIS2_PLACEMENT_3D('',#20527,#16382,#16383);
#14039=AXIS2_PLACEMENT_3D('',#20528,#16384,#16385);
#14040=AXIS2_PLACEMENT_3D('',#20531,#16386,#16387);
#14041=AXIS2_PLACEMENT_3D('',#20535,#16389,#16390);
#14042=AXIS2_PLACEMENT_3D('',#20537,#16392,#16393);
#14043=AXIS2_PLACEMENT_3D('',#20539,#16394,#16395);
#14044=AXIS2_PLACEMENT_3D('',#20542,#16397,#16398);
#14045=AXIS2_PLACEMENT_3D('',#20543,#16399,#16400);
#14046=AXIS2_PLACEMENT_3D('',#20550,#16404,#16405);
#14047=AXIS2_PLACEMENT_3D('',#20551,#16406,#16407);
#14048=AXIS2_PLACEMENT_3D('',#20560,#16412,#16413);
#14049=AXIS2_PLACEMENT_3D('',#20562,#16414,#16415);
#14050=AXIS2_PLACEMENT_3D('',#20564,#16416,#16417);
#14051=AXIS2_PLACEMENT_3D('',#20565,#16418,#16419);
#14052=AXIS2_PLACEMENT_3D('',#20567,#16420,#16421);
#14053=AXIS2_PLACEMENT_3D('',#20570,#16423,#16424);
#14054=AXIS2_PLACEMENT_3D('',#20571,#16425,#16426);
#14055=AXIS2_PLACEMENT_3D('',#20573,#16427,#16428);
#14056=AXIS2_PLACEMENT_3D('',#20574,#16429,#16430);
#14057=AXIS2_PLACEMENT_3D('',#20576,#16431,#16432);
#14058=AXIS2_PLACEMENT_3D('',#20578,#16434,#16435);
#14059=AXIS2_PLACEMENT_3D('',#20580,#16436,#16437);
#14060=AXIS2_PLACEMENT_3D('',#20582,#16439,#16440);
#14061=AXIS2_PLACEMENT_3D('',#20584,#16441,#16442);
#14062=AXIS2_PLACEMENT_3D('',#20585,#16443,#16444);
#14063=AXIS2_PLACEMENT_3D('',#20587,#16445,#16446);
#14064=AXIS2_PLACEMENT_3D('',#20589,#16448,#16449);
#14065=AXIS2_PLACEMENT_3D('',#20591,#16450,#16451);
#14066=AXIS2_PLACEMENT_3D('',#20593,#16453,#16454);
#14067=AXIS2_PLACEMENT_3D('',#20595,#16455,#16456);
#14068=AXIS2_PLACEMENT_3D('',#20597,#16458,#16459);
#14069=AXIS2_PLACEMENT_3D('',#20599,#16460,#16461);
#14070=AXIS2_PLACEMENT_3D('',#20601,#16463,#16464);
#14071=AXIS2_PLACEMENT_3D('',#20607,#16468,#16469);
#14072=AXIS2_PLACEMENT_3D('',#20611,#16472,#16473);
#14073=AXIS2_PLACEMENT_3D('',#20614,#16476,#16477);
#14074=AXIS2_PLACEMENT_3D('',#20615,#16478,#16479);
#14075=AXIS2_PLACEMENT_3D('',#20616,#16480,#16481);
#14076=AXIS2_PLACEMENT_3D('',#20617,#16482,#16483);
#14077=AXIS2_PLACEMENT_3D('',#20619,#16484,#16485);
#14078=AXIS2_PLACEMENT_3D('',#20622,#16487,#16488);
#14079=AXIS2_PLACEMENT_3D('',#20623,#16489,#16490);
#14080=AXIS2_PLACEMENT_3D('',#20625,#16491,#16492);
#14081=AXIS2_PLACEMENT_3D('',#20628,#16494,#16495);
#14082=AXIS2_PLACEMENT_3D('',#20629,#16496,#16497);
#14083=AXIS2_PLACEMENT_3D('',#20634,#16499,#16500);
#14084=AXIS2_PLACEMENT_3D('',#20637,#16502,#16503);
#14085=AXIS2_PLACEMENT_3D('',#20638,#16504,#16505);
#14086=AXIS2_PLACEMENT_3D('',#20643,#16507,#16508);
#14087=AXIS2_PLACEMENT_3D('',#20646,#16510,#16511);
#14088=AXIS2_PLACEMENT_3D('',#20647,#16512,#16513);
#14089=AXIS2_PLACEMENT_3D('',#20648,#16514,#16515);
#14090=AXIS2_PLACEMENT_3D('',#20649,#16516,#16517);
#14091=AXIS2_PLACEMENT_3D('',#20651,#16518,#16519);
#14092=AXIS2_PLACEMENT_3D('',#20652,#16520,#16521);
#14093=AXIS2_PLACEMENT_3D('',#20653,#16522,#16523);
#14094=AXIS2_PLACEMENT_3D('',#20654,#16524,#16525);
#14095=AXIS2_PLACEMENT_3D('',#20655,#16526,#16527);
#14096=AXIS2_PLACEMENT_3D('',#20656,#16528,#16529);
#14097=AXIS2_PLACEMENT_3D('',#20659,#16531,#16532);
#14098=AXIS2_PLACEMENT_3D('',#20660,#16533,#16534);
#14099=AXIS2_PLACEMENT_3D('',#20661,#16535,#16536);
#14100=AXIS2_PLACEMENT_3D('',#20662,#16537,#16538);
#14101=AXIS2_PLACEMENT_3D('',#20664,#16539,#16540);
#14102=AXIS2_PLACEMENT_3D('',#20666,#16541,#16542);
#14103=AXIS2_PLACEMENT_3D('',#20667,#16543,#16544);
#14104=AXIS2_PLACEMENT_3D('',#20670,#16546,#16547);
#14105=AXIS2_PLACEMENT_3D('',#20671,#16548,#16549);
#14106=AXIS2_PLACEMENT_3D('',#20672,#16550,#16551);
#14107=AXIS2_PLACEMENT_3D('',#20674,#16552,#16553);
#14108=AXIS2_PLACEMENT_3D('',#20676,#16555,#16556);
#14109=AXIS2_PLACEMENT_3D('',#20677,#16557,#16558);
#14110=AXIS2_PLACEMENT_3D('',#20678,#16559,#16560);
#14111=AXIS2_PLACEMENT_3D('',#20680,#16561,#16562);
#14112=AXIS2_PLACEMENT_3D('',#20682,#16563,#16564);
#14113=AXIS2_PLACEMENT_3D('',#20683,#16565,#16566);
#14114=AXIS2_PLACEMENT_3D('',#20686,#16568,#16569);
#14115=AXIS2_PLACEMENT_3D('',#20687,#16570,#16571);
#14116=AXIS2_PLACEMENT_3D('',#20688,#16572,#16573);
#14117=AXIS2_PLACEMENT_3D('',#20690,#16574,#16575);
#14118=AXIS2_PLACEMENT_3D('',#20692,#16577,#16578);
#14119=AXIS2_PLACEMENT_3D('',#20693,#16579,#16580);
#14120=AXIS2_PLACEMENT_3D('',#20694,#16581,#16582);
#14121=AXIS2_PLACEMENT_3D('',#20696,#16583,#16584);
#14122=AXIS2_PLACEMENT_3D('',#20699,#16586,#16587);
#14123=AXIS2_PLACEMENT_3D('',#20700,#16588,#16589);
#14124=AXIS2_PLACEMENT_3D('',#20702,#16590,#16591);
#14125=AXIS2_PLACEMENT_3D('',#20705,#16593,#16594);
#14126=AXIS2_PLACEMENT_3D('',#20706,#16595,#16596);
#14127=AXIS2_PLACEMENT_3D('',#20711,#16598,#16599);
#14128=AXIS2_PLACEMENT_3D('',#20714,#16601,#16602);
#14129=AXIS2_PLACEMENT_3D('',#20715,#16603,#16604);
#14130=AXIS2_PLACEMENT_3D('',#20720,#16606,#16607);
#14131=AXIS2_PLACEMENT_3D('',#20723,#16609,#16610);
#14132=AXIS2_PLACEMENT_3D('',#20724,#16611,#16612);
#14133=AXIS2_PLACEMENT_3D('',#20725,#16613,#16614);
#14134=AXIS2_PLACEMENT_3D('',#20726,#16615,#16616);
#14135=AXIS2_PLACEMENT_3D('',#20728,#16617,#16618);
#14136=AXIS2_PLACEMENT_3D('',#20729,#16619,#16620);
#14137=AXIS2_PLACEMENT_3D('',#20730,#16621,#16622);
#14138=AXIS2_PLACEMENT_3D('',#20731,#16623,#16624);
#14139=AXIS2_PLACEMENT_3D('',#20732,#16625,#16626);
#14140=AXIS2_PLACEMENT_3D('',#20733,#16627,#16628);
#14141=AXIS2_PLACEMENT_3D('',#20736,#16630,#16631);
#14142=AXIS2_PLACEMENT_3D('',#20737,#16632,#16633);
#14143=AXIS2_PLACEMENT_3D('',#20738,#16634,#16635);
#14144=AXIS2_PLACEMENT_3D('',#20739,#16636,#16637);
#14145=AXIS2_PLACEMENT_3D('',#20741,#16638,#16639);
#14146=AXIS2_PLACEMENT_3D('',#20743,#16640,#16641);
#14147=AXIS2_PLACEMENT_3D('',#20744,#16642,#16643);
#14148=AXIS2_PLACEMENT_3D('',#20746,#16644,#16645);
#14149=AXIS2_PLACEMENT_3D('',#20748,#16647,#16648);
#14150=AXIS2_PLACEMENT_3D('',#20749,#16649,#16650);
#14151=AXIS2_PLACEMENT_3D('',#20752,#16652,#16653);
#14152=AXIS2_PLACEMENT_3D('',#20753,#16654,#16655);
#14153=AXIS2_PLACEMENT_3D('',#20754,#16656,#16657);
#14154=AXIS2_PLACEMENT_3D('',#20755,#16658,#16659);
#14155=AXIS2_PLACEMENT_3D('',#20757,#16660,#16661);
#14156=AXIS2_PLACEMENT_3D('',#20759,#16662,#16663);
#14157=AXIS2_PLACEMENT_3D('',#20760,#16664,#16665);
#14158=AXIS2_PLACEMENT_3D('',#20762,#16666,#16667);
#14159=AXIS2_PLACEMENT_3D('',#20764,#16669,#16670);
#14160=AXIS2_PLACEMENT_3D('',#20765,#16671,#16672);
#14161=AXIS2_PLACEMENT_3D('',#20768,#16674,#16675);
#14162=AXIS2_PLACEMENT_3D('',#20769,#16676,#16677);
#14163=AXIS2_PLACEMENT_3D('',#20770,#16678,#16679);
#14164=AXIS2_PLACEMENT_3D('',#20771,#16680,#16681);
#14165=AXIS2_PLACEMENT_3D('',#20773,#16682,#16683);
#14166=AXIS2_PLACEMENT_3D('',#20776,#16685,#16686);
#14167=AXIS2_PLACEMENT_3D('',#20777,#16687,#16688);
#14168=AXIS2_PLACEMENT_3D('',#20778,#16689,#16690);
#14169=AXIS2_PLACEMENT_3D('',#20779,#16691,#16692);
#14170=AXIS2_PLACEMENT_3D('',#20780,#16693,#16694);
#14171=AXIS2_PLACEMENT_3D('',#20782,#16695,#16696);
#14172=AXIS2_PLACEMENT_3D('',#20785,#16698,#16699);
#14173=AXIS2_PLACEMENT_3D('',#20786,#16700,#16701);
#14174=AXIS2_PLACEMENT_3D('',#20787,#16702,#16703);
#14175=AXIS2_PLACEMENT_3D('',#20788,#16704,#16705);
#14176=AXIS2_PLACEMENT_3D('',#20789,#16706,#16707);
#14177=AXIS2_PLACEMENT_3D('',#20791,#16708,#16709);
#14178=AXIS2_PLACEMENT_3D('',#20792,#16710,#16711);
#14179=AXIS2_PLACEMENT_3D('',#20794,#16712,#16713);
#14180=AXIS2_PLACEMENT_3D('',#20796,#16715,#16716);
#14181=AXIS2_PLACEMENT_3D('',#20798,#16717,#16718);
#14182=AXIS2_PLACEMENT_3D('',#20800,#16720,#16721);
#14183=AXIS2_PLACEMENT_3D('',#20802,#16722,#16723);
#14184=AXIS2_PLACEMENT_3D('',#20804,#16725,#16726);
#14185=AXIS2_PLACEMENT_3D('',#20806,#16727,#16728);
#14186=AXIS2_PLACEMENT_3D('',#20807,#16729,#16730);
#14187=AXIS2_PLACEMENT_3D('',#20809,#16731,#16732);
#14188=AXIS2_PLACEMENT_3D('',#20811,#16734,#16735);
#14189=AXIS2_PLACEMENT_3D('',#20813,#16736,#16737);
#14190=AXIS2_PLACEMENT_3D('',#20815,#16739,#16740);
#14191=AXIS2_PLACEMENT_3D('',#20817,#16741,#16742);
#14192=AXIS2_PLACEMENT_3D('',#20819,#16744,#16745);
#14193=AXIS2_PLACEMENT_3D('',#20820,#16746,#16747);
#14194=AXIS2_PLACEMENT_3D('',#20829,#16752,#16753);
#14195=AXIS2_PLACEMENT_3D('',#20835,#16757,#16758);
#14196=AXIS2_PLACEMENT_3D('',#20841,#16762,#16763);
#14197=AXIS2_PLACEMENT_3D('',#20847,#16767,#16768);
#14198=AXIS2_PLACEMENT_3D('',#20853,#16772,#16773);
#14199=AXIS2_PLACEMENT_3D('',#20856,#16776,#16777);
#14200=AXIS2_PLACEMENT_3D('',#20857,#16778,#16779);
#14201=AXIS2_PLACEMENT_3D('',#20858,#16780,#16781);
#14202=AXIS2_PLACEMENT_3D('',#20859,#16782,#16783);
#14203=AXIS2_PLACEMENT_3D('',#20860,#16784,#16785);
#14204=AXIS2_PLACEMENT_3D('',#20862,#16786,#16787);
#14205=AXIS2_PLACEMENT_3D('',#20865,#16789,#16790);
#14206=AXIS2_PLACEMENT_3D('',#20866,#16791,#16792);
#14207=AXIS2_PLACEMENT_3D('',#20868,#16793,#16794);
#14208=AXIS2_PLACEMENT_3D('',#20871,#16796,#16797);
#14209=AXIS2_PLACEMENT_3D('',#20872,#16798,#16799);
#14210=AXIS2_PLACEMENT_3D('',#20874,#16800,#16801);
#14211=AXIS2_PLACEMENT_3D('',#20877,#16803,#16804);
#14212=AXIS2_PLACEMENT_3D('',#20878,#16805,#16806);
#14213=AXIS2_PLACEMENT_3D('',#20880,#16807,#16808);
#14214=AXIS2_PLACEMENT_3D('',#20883,#16810,#16811);
#14215=AXIS2_PLACEMENT_3D('',#20884,#16812,#16813);
#14216=AXIS2_PLACEMENT_3D('',#20886,#16814,#16815);
#14217=AXIS2_PLACEMENT_3D('',#20889,#16817,#16818);
#14218=AXIS2_PLACEMENT_3D('',#20890,#16819,#16820);
#14219=AXIS2_PLACEMENT_3D('',#20895,#16822,#16823);
#14220=AXIS2_PLACEMENT_3D('',#20898,#16825,#16826);
#14221=AXIS2_PLACEMENT_3D('',#20899,#16827,#16828);
#14222=AXIS2_PLACEMENT_3D('',#20903,#16830,#16831);
#14223=AXIS2_PLACEMENT_3D('',#20906,#16833,#16834);
#14224=AXIS2_PLACEMENT_3D('',#20908,#16835,#16836);
#14225=AXIS2_PLACEMENT_3D('',#20910,#16837,#16838);
#14226=AXIS2_PLACEMENT_3D('',#20912,#16839,#16840);
#14227=AXIS2_PLACEMENT_3D('',#20914,#16841,#16842);
#14228=AXIS2_PLACEMENT_3D('',#20915,#16843,#16844);
#14229=AXIS2_PLACEMENT_3D('',#20919,#16847,#16848);
#14230=AXIS2_PLACEMENT_3D('',#20922,#16850,#16851);
#14231=AXIS2_PLACEMENT_3D('',#20923,#16852,#16853);
#14232=AXIS2_PLACEMENT_3D('',#20926,#16855,#16856);
#14233=AXIS2_PLACEMENT_3D('',#20927,#16857,#16858);
#14234=AXIS2_PLACEMENT_3D('',#20930,#16860,#16861);
#14235=AXIS2_PLACEMENT_3D('',#20931,#16862,#16863);
#14236=AXIS2_PLACEMENT_3D('',#20934,#16865,#16866);
#14237=AXIS2_PLACEMENT_3D('',#20935,#16867,#16868);
#14238=AXIS2_PLACEMENT_3D('',#20938,#16870,#16871);
#14239=AXIS2_PLACEMENT_3D('',#20939,#16872,#16873);
#14240=AXIS2_PLACEMENT_3D('',#20942,#16875,#16876);
#14241=AXIS2_PLACEMENT_3D('',#20943,#16877,#16878);
#14242=AXIS2_PLACEMENT_3D('',#20945,#16880,#16881);
#14243=AXIS2_PLACEMENT_3D('',#20946,#16882,#16883);
#14244=AXIS2_PLACEMENT_3D('',#20947,#16884,#16885);
#14245=AXIS2_PLACEMENT_3D('',#20949,#16886,#16887);
#14246=AXIS2_PLACEMENT_3D('',#20952,#16889,#16890);
#14247=AXIS2_PLACEMENT_3D('',#20953,#16891,#16892);
#14248=AXIS2_PLACEMENT_3D('',#20955,#16893,#16894);
#14249=AXIS2_PLACEMENT_3D('',#20958,#16896,#16897);
#14250=AXIS2_PLACEMENT_3D('',#20959,#16898,#16899);
#14251=AXIS2_PLACEMENT_3D('',#20961,#16900,#16901);
#14252=AXIS2_PLACEMENT_3D('',#20964,#16903,#16904);
#14253=AXIS2_PLACEMENT_3D('',#20965,#16905,#16906);
#14254=AXIS2_PLACEMENT_3D('',#20967,#16907,#16908);
#14255=AXIS2_PLACEMENT_3D('',#20970,#16910,#16911);
#14256=AXIS2_PLACEMENT_3D('',#20971,#16912,#16913);
#14257=AXIS2_PLACEMENT_3D('',#20973,#16914,#16915);
#14258=AXIS2_PLACEMENT_3D('',#20976,#16917,#16918);
#14259=AXIS2_PLACEMENT_3D('',#20977,#16919,#16920);
#14260=AXIS2_PLACEMENT_3D('',#20979,#16921,#16922);
#14261=AXIS2_PLACEMENT_3D('',#20982,#16924,#16925);
#14262=AXIS2_PLACEMENT_3D('',#20983,#16926,#16927);
#14263=AXIS2_PLACEMENT_3D('',#20984,#16928,#16929);
#14264=AXIS2_PLACEMENT_3D('',#20985,#16930,#16931);
#14265=AXIS2_PLACEMENT_3D('',#20986,#16932,#16933);
#14266=AXIS2_PLACEMENT_3D('',#20988,#16934,#16935);
#14267=AXIS2_PLACEMENT_3D('',#20990,#16936,#16937);
#14268=AXIS2_PLACEMENT_3D('',#20991,#16938,#16939);
#14269=AXIS2_PLACEMENT_3D('',#20994,#16941,#16942);
#14270=AXIS2_PLACEMENT_3D('',#20995,#16943,#16944);
#14271=AXIS2_PLACEMENT_3D('',#20996,#16945,#16946);
#14272=AXIS2_PLACEMENT_3D('',#20998,#16947,#16948);
#14273=AXIS2_PLACEMENT_3D('',#21000,#16950,#16951);
#14274=AXIS2_PLACEMENT_3D('',#21001,#16952,#16953);
#14275=AXIS2_PLACEMENT_3D('',#21002,#16954,#16955);
#14276=AXIS2_PLACEMENT_3D('',#21004,#16956,#16957);
#14277=AXIS2_PLACEMENT_3D('',#21006,#16958,#16959);
#14278=AXIS2_PLACEMENT_3D('',#21007,#16960,#16961);
#14279=AXIS2_PLACEMENT_3D('',#21010,#16963,#16964);
#14280=AXIS2_PLACEMENT_3D('',#21011,#16965,#16966);
#14281=AXIS2_PLACEMENT_3D('',#21012,#16967,#16968);
#14282=AXIS2_PLACEMENT_3D('',#21014,#16969,#16970);
#14283=AXIS2_PLACEMENT_3D('',#21016,#16972,#16973);
#14284=AXIS2_PLACEMENT_3D('',#21017,#16974,#16975);
#14285=AXIS2_PLACEMENT_3D('',#21018,#16976,#16977);
#14286=AXIS2_PLACEMENT_3D('',#21020,#16978,#16979);
#14287=AXIS2_PLACEMENT_3D('',#21022,#16980,#16981);
#14288=AXIS2_PLACEMENT_3D('',#21023,#16982,#16983);
#14289=AXIS2_PLACEMENT_3D('',#21026,#16985,#16986);
#14290=AXIS2_PLACEMENT_3D('',#21027,#16987,#16988);
#14291=AXIS2_PLACEMENT_3D('',#21028,#16989,#16990);
#14292=AXIS2_PLACEMENT_3D('',#21030,#16991,#16992);
#14293=AXIS2_PLACEMENT_3D('',#21032,#16994,#16995);
#14294=AXIS2_PLACEMENT_3D('',#21033,#16996,#16997);
#14295=AXIS2_PLACEMENT_3D('',#21034,#16998,#16999);
#14296=AXIS2_PLACEMENT_3D('',#21036,#17000,#17001);
#14297=AXIS2_PLACEMENT_3D('',#21038,#17002,#17003);
#14298=AXIS2_PLACEMENT_3D('',#21039,#17004,#17005);
#14299=AXIS2_PLACEMENT_3D('',#21042,#17007,#17008);
#14300=AXIS2_PLACEMENT_3D('',#21043,#17009,#17010);
#14301=AXIS2_PLACEMENT_3D('',#21044,#17011,#17012);
#14302=AXIS2_PLACEMENT_3D('',#21046,#17013,#17014);
#14303=AXIS2_PLACEMENT_3D('',#21048,#17016,#17017);
#14304=AXIS2_PLACEMENT_3D('',#21049,#17018,#17019);
#14305=AXIS2_PLACEMENT_3D('',#21050,#17020,#17021);
#14306=AXIS2_PLACEMENT_3D('',#21052,#17022,#17023);
#14307=AXIS2_PLACEMENT_3D('',#21055,#17025,#17026);
#14308=AXIS2_PLACEMENT_3D('',#21056,#17027,#17028);
#14309=AXIS2_PLACEMENT_3D('',#21058,#17029,#17030);
#14310=AXIS2_PLACEMENT_3D('',#21061,#17032,#17033);
#14311=AXIS2_PLACEMENT_3D('',#21062,#17034,#17035);
#14312=AXIS2_PLACEMENT_3D('',#21064,#17036,#17037);
#14313=AXIS2_PLACEMENT_3D('',#21067,#17039,#17040);
#14314=AXIS2_PLACEMENT_3D('',#21068,#17041,#17042);
#14315=AXIS2_PLACEMENT_3D('',#21070,#17043,#17044);
#14316=AXIS2_PLACEMENT_3D('',#21073,#17046,#17047);
#14317=AXIS2_PLACEMENT_3D('',#21074,#17048,#17049);
#14318=AXIS2_PLACEMENT_3D('',#21076,#17050,#17051);
#14319=AXIS2_PLACEMENT_3D('',#21079,#17053,#17054);
#14320=AXIS2_PLACEMENT_3D('',#21080,#17055,#17056);
#14321=AXIS2_PLACEMENT_3D('',#21082,#17057,#17058);
#14322=AXIS2_PLACEMENT_3D('',#21085,#17060,#17061);
#14323=AXIS2_PLACEMENT_3D('',#21086,#17062,#17063);
#14324=AXIS2_PLACEMENT_3D('',#21087,#17064,#17065);
#14325=AXIS2_PLACEMENT_3D('',#21088,#17066,#17067);
#14326=AXIS2_PLACEMENT_3D('',#21089,#17068,#17069);
#14327=AXIS2_PLACEMENT_3D('',#21091,#17070,#17071);
#14328=AXIS2_PLACEMENT_3D('',#21093,#17072,#17073);
#14329=AXIS2_PLACEMENT_3D('',#21094,#17074,#17075);
#14330=AXIS2_PLACEMENT_3D('',#21096,#17076,#17077);
#14331=AXIS2_PLACEMENT_3D('',#21098,#17079,#17080);
#14332=AXIS2_PLACEMENT_3D('',#21099,#17081,#17082);
#14333=AXIS2_PLACEMENT_3D('',#21102,#17084,#17085);
#14334=AXIS2_PLACEMENT_3D('',#21103,#17086,#17087);
#14335=AXIS2_PLACEMENT_3D('',#21104,#17088,#17089);
#14336=AXIS2_PLACEMENT_3D('',#21105,#17090,#17091);
#14337=AXIS2_PLACEMENT_3D('',#21107,#17092,#17093);
#14338=AXIS2_PLACEMENT_3D('',#21109,#17094,#17095);
#14339=AXIS2_PLACEMENT_3D('',#21110,#17096,#17097);
#14340=AXIS2_PLACEMENT_3D('',#21112,#17098,#17099);
#14341=AXIS2_PLACEMENT_3D('',#21114,#17101,#17102);
#14342=AXIS2_PLACEMENT_3D('',#21115,#17103,#17104);
#14343=AXIS2_PLACEMENT_3D('',#21118,#17106,#17107);
#14344=AXIS2_PLACEMENT_3D('',#21119,#17108,#17109);
#14345=AXIS2_PLACEMENT_3D('',#21120,#17110,#17111);
#14346=AXIS2_PLACEMENT_3D('',#21121,#17112,#17113);
#14347=AXIS2_PLACEMENT_3D('',#21123,#17114,#17115);
#14348=AXIS2_PLACEMENT_3D('',#21125,#17116,#17117);
#14349=AXIS2_PLACEMENT_3D('',#21126,#17118,#17119);
#14350=AXIS2_PLACEMENT_3D('',#21128,#17120,#17121);
#14351=AXIS2_PLACEMENT_3D('',#21130,#17123,#17124);
#14352=AXIS2_PLACEMENT_3D('',#21131,#17125,#17126);
#14353=AXIS2_PLACEMENT_3D('',#21134,#17128,#17129);
#14354=AXIS2_PLACEMENT_3D('',#21135,#17130,#17131);
#14355=AXIS2_PLACEMENT_3D('',#21136,#17132,#17133);
#14356=AXIS2_PLACEMENT_3D('',#21137,#17134,#17135);
#14357=AXIS2_PLACEMENT_3D('',#21139,#17136,#17137);
#14358=AXIS2_PLACEMENT_3D('',#21141,#17138,#17139);
#14359=AXIS2_PLACEMENT_3D('',#21142,#17140,#17141);
#14360=AXIS2_PLACEMENT_3D('',#21144,#17142,#17143);
#14361=AXIS2_PLACEMENT_3D('',#21146,#17145,#17146);
#14362=AXIS2_PLACEMENT_3D('',#21147,#17147,#17148);
#14363=AXIS2_PLACEMENT_3D('',#21150,#17150,#17151);
#14364=AXIS2_PLACEMENT_3D('',#21151,#17152,#17153);
#14365=AXIS2_PLACEMENT_3D('',#21152,#17154,#17155);
#14366=AXIS2_PLACEMENT_3D('',#21153,#17156,#17157);
#14367=AXIS2_PLACEMENT_3D('',#21155,#17158,#17159);
#14368=AXIS2_PLACEMENT_3D('',#21158,#17161,#17162);
#14369=AXIS2_PLACEMENT_3D('',#21159,#17163,#17164);
#14370=AXIS2_PLACEMENT_3D('',#21161,#17165,#17166);
#14371=AXIS2_PLACEMENT_3D('',#21164,#17168,#17169);
#14372=AXIS2_PLACEMENT_3D('',#21165,#17170,#17171);
#14373=AXIS2_PLACEMENT_3D('',#21167,#17172,#17173);
#14374=AXIS2_PLACEMENT_3D('',#21170,#17175,#17176);
#14375=AXIS2_PLACEMENT_3D('',#21171,#17177,#17178);
#14376=AXIS2_PLACEMENT_3D('',#21173,#17179,#17180);
#14377=AXIS2_PLACEMENT_3D('',#21176,#17182,#17183);
#14378=AXIS2_PLACEMENT_3D('',#21177,#17184,#17185);
#14379=AXIS2_PLACEMENT_3D('',#21179,#17186,#17187);
#14380=AXIS2_PLACEMENT_3D('',#21182,#17189,#17190);
#14381=AXIS2_PLACEMENT_3D('',#21183,#17191,#17192);
#14382=AXIS2_PLACEMENT_3D('',#21185,#17193,#17194);
#14383=AXIS2_PLACEMENT_3D('',#21188,#17196,#17197);
#14384=AXIS2_PLACEMENT_3D('',#21189,#17198,#17199);
#14385=AXIS2_PLACEMENT_3D('',#21190,#17200,#17201);
#14386=AXIS2_PLACEMENT_3D('',#21191,#17202,#17203);
#14387=AXIS2_PLACEMENT_3D('',#21192,#17204,#17205);
#14388=AXIS2_PLACEMENT_3D('',#21194,#17206,#17207);
#14389=AXIS2_PLACEMENT_3D('',#21196,#17208,#17209);
#14390=AXIS2_PLACEMENT_3D('',#21197,#17210,#17211);
#14391=AXIS2_PLACEMENT_3D('',#21200,#17213,#17214);
#14392=AXIS2_PLACEMENT_3D('',#21201,#17215,#17216);
#14393=AXIS2_PLACEMENT_3D('',#21202,#17217,#17218);
#14394=AXIS2_PLACEMENT_3D('',#21204,#17219,#17220);
#14395=AXIS2_PLACEMENT_3D('',#21206,#17222,#17223);
#14396=AXIS2_PLACEMENT_3D('',#21207,#17224,#17225);
#14397=AXIS2_PLACEMENT_3D('',#21208,#17226,#17227);
#14398=AXIS2_PLACEMENT_3D('',#21210,#17228,#17229);
#14399=AXIS2_PLACEMENT_3D('',#21212,#17230,#17231);
#14400=AXIS2_PLACEMENT_3D('',#21213,#17232,#17233);
#14401=AXIS2_PLACEMENT_3D('',#21216,#17235,#17236);
#14402=AXIS2_PLACEMENT_3D('',#21217,#17237,#17238);
#14403=AXIS2_PLACEMENT_3D('',#21218,#17239,#17240);
#14404=AXIS2_PLACEMENT_3D('',#21220,#17241,#17242);
#14405=AXIS2_PLACEMENT_3D('',#21222,#17244,#17245);
#14406=AXIS2_PLACEMENT_3D('',#21223,#17246,#17247);
#14407=AXIS2_PLACEMENT_3D('',#21224,#17248,#17249);
#14408=AXIS2_PLACEMENT_3D('',#21226,#17250,#17251);
#14409=AXIS2_PLACEMENT_3D('',#21228,#17252,#17253);
#14410=AXIS2_PLACEMENT_3D('',#21229,#17254,#17255);
#14411=AXIS2_PLACEMENT_3D('',#21232,#17257,#17258);
#14412=AXIS2_PLACEMENT_3D('',#21233,#17259,#17260);
#14413=AXIS2_PLACEMENT_3D('',#21234,#17261,#17262);
#14414=AXIS2_PLACEMENT_3D('',#21236,#17263,#17264);
#14415=AXIS2_PLACEMENT_3D('',#21238,#17266,#17267);
#14416=AXIS2_PLACEMENT_3D('',#21239,#17268,#17269);
#14417=AXIS2_PLACEMENT_3D('',#21240,#17270,#17271);
#14418=AXIS2_PLACEMENT_3D('',#21242,#17272,#17273);
#14419=AXIS2_PLACEMENT_3D('',#21244,#17274,#17275);
#14420=AXIS2_PLACEMENT_3D('',#21245,#17276,#17277);
#14421=AXIS2_PLACEMENT_3D('',#21248,#17279,#17280);
#14422=AXIS2_PLACEMENT_3D('',#21249,#17281,#17282);
#14423=AXIS2_PLACEMENT_3D('',#21250,#17283,#17284);
#14424=AXIS2_PLACEMENT_3D('',#21252,#17285,#17286);
#14425=AXIS2_PLACEMENT_3D('',#21254,#17288,#17289);
#14426=AXIS2_PLACEMENT_3D('',#21255,#17290,#17291);
#14427=AXIS2_PLACEMENT_3D('',#21256,#17292,#17293);
#14428=AXIS2_PLACEMENT_3D('',#21258,#17294,#17295);
#14429=AXIS2_PLACEMENT_3D('',#21261,#17297,#17298);
#14430=AXIS2_PLACEMENT_3D('',#21262,#17299,#17300);
#14431=AXIS2_PLACEMENT_3D('',#21264,#17301,#17302);
#14432=AXIS2_PLACEMENT_3D('',#21267,#17304,#17305);
#14433=AXIS2_PLACEMENT_3D('',#21268,#17306,#17307);
#14434=AXIS2_PLACEMENT_3D('',#21270,#17308,#17309);
#14435=AXIS2_PLACEMENT_3D('',#21273,#17311,#17312);
#14436=AXIS2_PLACEMENT_3D('',#21274,#17313,#17314);
#14437=AXIS2_PLACEMENT_3D('',#21276,#17315,#17316);
#14438=AXIS2_PLACEMENT_3D('',#21279,#17318,#17319);
#14439=AXIS2_PLACEMENT_3D('',#21280,#17320,#17321);
#14440=AXIS2_PLACEMENT_3D('',#21282,#17322,#17323);
#14441=AXIS2_PLACEMENT_3D('',#21285,#17325,#17326);
#14442=AXIS2_PLACEMENT_3D('',#21286,#17327,#17328);
#14443=AXIS2_PLACEMENT_3D('',#21288,#17329,#17330);
#14444=AXIS2_PLACEMENT_3D('',#21291,#17332,#17333);
#14445=AXIS2_PLACEMENT_3D('',#21292,#17334,#17335);
#14446=AXIS2_PLACEMENT_3D('',#21293,#17336,#17337);
#14447=AXIS2_PLACEMENT_3D('',#21294,#17338,#17339);
#14448=AXIS2_PLACEMENT_3D('',#21295,#17340,#17341);
#14449=AXIS2_PLACEMENT_3D('',#21297,#17342,#17343);
#14450=AXIS2_PLACEMENT_3D('',#21299,#17344,#17345);
#14451=AXIS2_PLACEMENT_3D('',#21300,#17346,#17347);
#14452=AXIS2_PLACEMENT_3D('',#21302,#17348,#17349);
#14453=AXIS2_PLACEMENT_3D('',#21304,#17351,#17352);
#14454=AXIS2_PLACEMENT_3D('',#21305,#17353,#17354);
#14455=AXIS2_PLACEMENT_3D('',#21308,#17356,#17357);
#14456=AXIS2_PLACEMENT_3D('',#21309,#17358,#17359);
#14457=AXIS2_PLACEMENT_3D('',#21310,#17360,#17361);
#14458=AXIS2_PLACEMENT_3D('',#21311,#17362,#17363);
#14459=AXIS2_PLACEMENT_3D('',#21313,#17364,#17365);
#14460=AXIS2_PLACEMENT_3D('',#21315,#17366,#17367);
#14461=AXIS2_PLACEMENT_3D('',#21316,#17368,#17369);
#14462=AXIS2_PLACEMENT_3D('',#21318,#17370,#17371);
#14463=AXIS2_PLACEMENT_3D('',#21320,#17373,#17374);
#14464=AXIS2_PLACEMENT_3D('',#21321,#17375,#17376);
#14465=AXIS2_PLACEMENT_3D('',#21324,#17378,#17379);
#14466=AXIS2_PLACEMENT_3D('',#21325,#17380,#17381);
#14467=AXIS2_PLACEMENT_3D('',#21326,#17382,#17383);
#14468=AXIS2_PLACEMENT_3D('',#21327,#17384,#17385);
#14469=AXIS2_PLACEMENT_3D('',#21329,#17386,#17387);
#14470=AXIS2_PLACEMENT_3D('',#21331,#17388,#17389);
#14471=AXIS2_PLACEMENT_3D('',#21332,#17390,#17391);
#14472=AXIS2_PLACEMENT_3D('',#21334,#17392,#17393);
#14473=AXIS2_PLACEMENT_3D('',#21336,#17395,#17396);
#14474=AXIS2_PLACEMENT_3D('',#21337,#17397,#17398);
#14475=AXIS2_PLACEMENT_3D('',#21340,#17400,#17401);
#14476=AXIS2_PLACEMENT_3D('',#21341,#17402,#17403);
#14477=AXIS2_PLACEMENT_3D('',#21342,#17404,#17405);
#14478=AXIS2_PLACEMENT_3D('',#21343,#17406,#17407);
#14479=AXIS2_PLACEMENT_3D('',#21345,#17408,#17409);
#14480=AXIS2_PLACEMENT_3D('',#21347,#17410,#17411);
#14481=AXIS2_PLACEMENT_3D('',#21348,#17412,#17413);
#14482=AXIS2_PLACEMENT_3D('',#21350,#17414,#17415);
#14483=AXIS2_PLACEMENT_3D('',#21352,#17417,#17418);
#14484=AXIS2_PLACEMENT_3D('',#21353,#17419,#17420);
#14485=AXIS2_PLACEMENT_3D('',#21356,#17422,#17423);
#14486=AXIS2_PLACEMENT_3D('',#21357,#17424,#17425);
#14487=AXIS2_PLACEMENT_3D('',#21358,#17426,#17427);
#14488=AXIS2_PLACEMENT_3D('',#21359,#17428,#17429);
#14489=AXIS2_PLACEMENT_3D('',#21360,#17430,#17431);
#14490=AXIS2_PLACEMENT_3D('',#21362,#17432,#17433);
#14491=AXIS2_PLACEMENT_3D('',#21365,#17435,#17436);
#14492=AXIS2_PLACEMENT_3D('',#21366,#17437,#17438);
#14493=AXIS2_PLACEMENT_3D('',#21368,#17439,#17440);
#14494=AXIS2_PLACEMENT_3D('',#21371,#17442,#17443);
#14495=AXIS2_PLACEMENT_3D('',#21372,#17444,#17445);
#14496=AXIS2_PLACEMENT_3D('',#21374,#17446,#17447);
#14497=AXIS2_PLACEMENT_3D('',#21377,#17449,#17450);
#14498=AXIS2_PLACEMENT_3D('',#21378,#17451,#17452);
#14499=AXIS2_PLACEMENT_3D('',#21380,#17453,#17454);
#14500=AXIS2_PLACEMENT_3D('',#21383,#17456,#17457);
#14501=AXIS2_PLACEMENT_3D('',#21384,#17458,#17459);
#14502=AXIS2_PLACEMENT_3D('',#21386,#17460,#17461);
#14503=AXIS2_PLACEMENT_3D('',#21389,#17463,#17464);
#14504=AXIS2_PLACEMENT_3D('',#21390,#17465,#17466);
#14505=AXIS2_PLACEMENT_3D('',#21395,#17468,#17469);
#14506=AXIS2_PLACEMENT_3D('',#21398,#17471,#17472);
#14507=AXIS2_PLACEMENT_3D('',#21399,#17473,#17474);
#14508=AXIS2_PLACEMENT_3D('',#21405,#17478,#17479);
#14509=AXIS2_PLACEMENT_3D('',#21408,#17481,#17482);
#14510=AXIS2_PLACEMENT_3D('',#21410,#17483,#17484);
#14511=AXIS2_PLACEMENT_3D('',#21412,#17485,#17486);
#14512=AXIS2_PLACEMENT_3D('',#21414,#17487,#17488);
#14513=AXIS2_PLACEMENT_3D('',#21416,#17489,#17490);
#14514=AXIS2_PLACEMENT_3D('',#21418,#17491,#17492);
#14515=AXIS2_PLACEMENT_3D('',#21419,#17493,#17494);
#14516=AXIS2_PLACEMENT_3D('',#21421,#17495,#17496);
#14517=AXIS2_PLACEMENT_3D('',#21423,#17498,#17499);
#14518=AXIS2_PLACEMENT_3D('',#21425,#17500,#17501);
#14519=AXIS2_PLACEMENT_3D('',#21427,#17503,#17504);
#14520=AXIS2_PLACEMENT_3D('',#21429,#17505,#17506);
#14521=AXIS2_PLACEMENT_3D('',#21431,#17508,#17509);
#14522=AXIS2_PLACEMENT_3D('',#21433,#17510,#17511);
#14523=AXIS2_PLACEMENT_3D('',#21435,#17513,#17514);
#14524=AXIS2_PLACEMENT_3D('',#21437,#17515,#17516);
#14525=AXIS2_PLACEMENT_3D('',#21439,#17518,#17519);
#14526=AXIS2_PLACEMENT_3D('',#21442,#17521,#17522);
#14527=AXIS2_PLACEMENT_3D('',#21443,#17523,#17524);
#14528=AXIS2_PLACEMENT_3D('',#21445,#17526,#17527);
#14529=AXIS2_PLACEMENT_3D('',#21446,#17528,#17529);
#14530=AXIS2_PLACEMENT_3D('',#21447,#17530,#17531);
#14531=AXIS2_PLACEMENT_3D('',#21449,#17532,#17533);
#14532=AXIS2_PLACEMENT_3D('',#21452,#17535,#17536);
#14533=AXIS2_PLACEMENT_3D('',#21453,#17537,#17538);
#14534=AXIS2_PLACEMENT_3D('',#21455,#17539,#17540);
#14535=AXIS2_PLACEMENT_3D('',#21458,#17542,#17543);
#14536=AXIS2_PLACEMENT_3D('',#21459,#17544,#17545);
#14537=AXIS2_PLACEMENT_3D('',#21461,#17546,#17547);
#14538=AXIS2_PLACEMENT_3D('',#21464,#17549,#17550);
#14539=AXIS2_PLACEMENT_3D('',#21465,#17551,#17552);
#14540=AXIS2_PLACEMENT_3D('',#21467,#17553,#17554);
#14541=AXIS2_PLACEMENT_3D('',#21470,#17556,#17557);
#14542=AXIS2_PLACEMENT_3D('',#21471,#17558,#17559);
#14543=AXIS2_PLACEMENT_3D('',#21473,#17560,#17561);
#14544=AXIS2_PLACEMENT_3D('',#21476,#17563,#17564);
#14545=AXIS2_PLACEMENT_3D('',#21477,#17565,#17566);
#14546=AXIS2_PLACEMENT_3D('',#21479,#17567,#17568);
#14547=AXIS2_PLACEMENT_3D('',#21482,#17570,#17571);
#14548=AXIS2_PLACEMENT_3D('',#21483,#17572,#17573);
#14549=AXIS2_PLACEMENT_3D('',#21484,#17574,#17575);
#14550=AXIS2_PLACEMENT_3D('',#21485,#17576,#17577);
#14551=AXIS2_PLACEMENT_3D('',#21486,#17578,#17579);
#14552=AXIS2_PLACEMENT_3D('',#21488,#17580,#17581);
#14553=AXIS2_PLACEMENT_3D('',#21490,#17582,#17583);
#14554=AXIS2_PLACEMENT_3D('',#21491,#17584,#17585);
#14555=AXIS2_PLACEMENT_3D('',#21494,#17587,#17588);
#14556=AXIS2_PLACEMENT_3D('',#21495,#17589,#17590);
#14557=AXIS2_PLACEMENT_3D('',#21496,#17591,#17592);
#14558=AXIS2_PLACEMENT_3D('',#21498,#17593,#17594);
#14559=AXIS2_PLACEMENT_3D('',#21500,#17596,#17597);
#14560=AXIS2_PLACEMENT_3D('',#21501,#17598,#17599);
#14561=AXIS2_PLACEMENT_3D('',#21502,#17600,#17601);
#14562=AXIS2_PLACEMENT_3D('',#21504,#17602,#17603);
#14563=AXIS2_PLACEMENT_3D('',#21506,#17604,#17605);
#14564=AXIS2_PLACEMENT_3D('',#21507,#17606,#17607);
#14565=AXIS2_PLACEMENT_3D('',#21510,#17609,#17610);
#14566=AXIS2_PLACEMENT_3D('',#21511,#17611,#17612);
#14567=AXIS2_PLACEMENT_3D('',#21512,#17613,#17614);
#14568=AXIS2_PLACEMENT_3D('',#21514,#17615,#17616);
#14569=AXIS2_PLACEMENT_3D('',#21516,#17618,#17619);
#14570=AXIS2_PLACEMENT_3D('',#21517,#17620,#17621);
#14571=AXIS2_PLACEMENT_3D('',#21518,#17622,#17623);
#14572=AXIS2_PLACEMENT_3D('',#21520,#17624,#17625);
#14573=AXIS2_PLACEMENT_3D('',#21522,#17626,#17627);
#14574=AXIS2_PLACEMENT_3D('',#21523,#17628,#17629);
#14575=AXIS2_PLACEMENT_3D('',#21526,#17631,#17632);
#14576=AXIS2_PLACEMENT_3D('',#21527,#17633,#17634);
#14577=AXIS2_PLACEMENT_3D('',#21528,#17635,#17636);
#14578=AXIS2_PLACEMENT_3D('',#21530,#17637,#17638);
#14579=AXIS2_PLACEMENT_3D('',#21532,#17640,#17641);
#14580=AXIS2_PLACEMENT_3D('',#21533,#17642,#17643);
#14581=AXIS2_PLACEMENT_3D('',#21534,#17644,#17645);
#14582=AXIS2_PLACEMENT_3D('',#21536,#17646,#17647);
#14583=AXIS2_PLACEMENT_3D('',#21538,#17648,#17649);
#14584=AXIS2_PLACEMENT_3D('',#21539,#17650,#17651);
#14585=AXIS2_PLACEMENT_3D('',#21542,#17653,#17654);
#14586=AXIS2_PLACEMENT_3D('',#21543,#17655,#17656);
#14587=AXIS2_PLACEMENT_3D('',#21544,#17657,#17658);
#14588=AXIS2_PLACEMENT_3D('',#21546,#17659,#17660);
#14589=AXIS2_PLACEMENT_3D('',#21548,#17662,#17663);
#14590=AXIS2_PLACEMENT_3D('',#21549,#17664,#17665);
#14591=AXIS2_PLACEMENT_3D('',#21550,#17666,#17667);
#14592=AXIS2_PLACEMENT_3D('',#21552,#17668,#17669);
#14593=AXIS2_PLACEMENT_3D('',#21555,#17671,#17672);
#14594=AXIS2_PLACEMENT_3D('',#21556,#17673,#17674);
#14595=AXIS2_PLACEMENT_3D('',#21558,#17675,#17676);
#14596=AXIS2_PLACEMENT_3D('',#21561,#17678,#17679);
#14597=AXIS2_PLACEMENT_3D('',#21562,#17680,#17681);
#14598=AXIS2_PLACEMENT_3D('',#21564,#17682,#17683);
#14599=AXIS2_PLACEMENT_3D('',#21567,#17685,#17686);
#14600=AXIS2_PLACEMENT_3D('',#21568,#17687,#17688);
#14601=AXIS2_PLACEMENT_3D('',#21570,#17689,#17690);
#14602=AXIS2_PLACEMENT_3D('',#21573,#17692,#17693);
#14603=AXIS2_PLACEMENT_3D('',#21574,#17694,#17695);
#14604=AXIS2_PLACEMENT_3D('',#21576,#17696,#17697);
#14605=AXIS2_PLACEMENT_3D('',#21579,#17699,#17700);
#14606=AXIS2_PLACEMENT_3D('',#21580,#17701,#17702);
#14607=AXIS2_PLACEMENT_3D('',#21582,#17703,#17704);
#14608=AXIS2_PLACEMENT_3D('',#21585,#17706,#17707);
#14609=AXIS2_PLACEMENT_3D('',#21586,#17708,#17709);
#14610=AXIS2_PLACEMENT_3D('',#21587,#17710,#17711);
#14611=AXIS2_PLACEMENT_3D('',#21588,#17712,#17713);
#14612=AXIS2_PLACEMENT_3D('',#21589,#17714,#17715);
#14613=AXIS2_PLACEMENT_3D('',#21591,#17716,#17717);
#14614=AXIS2_PLACEMENT_3D('',#21593,#17718,#17719);
#14615=AXIS2_PLACEMENT_3D('',#21594,#17720,#17721);
#14616=AXIS2_PLACEMENT_3D('',#21596,#17722,#17723);
#14617=AXIS2_PLACEMENT_3D('',#21598,#17725,#17726);
#14618=AXIS2_PLACEMENT_3D('',#21599,#17727,#17728);
#14619=AXIS2_PLACEMENT_3D('',#21602,#17730,#17731);
#14620=AXIS2_PLACEMENT_3D('',#21603,#17732,#17733);
#14621=AXIS2_PLACEMENT_3D('',#21604,#17734,#17735);
#14622=AXIS2_PLACEMENT_3D('',#21605,#17736,#17737);
#14623=AXIS2_PLACEMENT_3D('',#21607,#17738,#17739);
#14624=AXIS2_PLACEMENT_3D('',#21609,#17740,#17741);
#14625=AXIS2_PLACEMENT_3D('',#21610,#17742,#17743);
#14626=AXIS2_PLACEMENT_3D('',#21612,#17744,#17745);
#14627=AXIS2_PLACEMENT_3D('',#21614,#17747,#17748);
#14628=AXIS2_PLACEMENT_3D('',#21615,#17749,#17750);
#14629=AXIS2_PLACEMENT_3D('',#21618,#17752,#17753);
#14630=AXIS2_PLACEMENT_3D('',#21619,#17754,#17755);
#14631=AXIS2_PLACEMENT_3D('',#21620,#17756,#17757);
#14632=AXIS2_PLACEMENT_3D('',#21621,#17758,#17759);
#14633=AXIS2_PLACEMENT_3D('',#21623,#17760,#17761);
#14634=AXIS2_PLACEMENT_3D('',#21625,#17762,#17763);
#14635=AXIS2_PLACEMENT_3D('',#21626,#17764,#17765);
#14636=AXIS2_PLACEMENT_3D('',#21628,#17766,#17767);
#14637=AXIS2_PLACEMENT_3D('',#21630,#17769,#17770);
#14638=AXIS2_PLACEMENT_3D('',#21631,#17771,#17772);
#14639=AXIS2_PLACEMENT_3D('',#21634,#17774,#17775);
#14640=AXIS2_PLACEMENT_3D('',#21635,#17776,#17777);
#14641=AXIS2_PLACEMENT_3D('',#21636,#17778,#17779);
#14642=AXIS2_PLACEMENT_3D('',#21637,#17780,#17781);
#14643=AXIS2_PLACEMENT_3D('',#21639,#17782,#17783);
#14644=AXIS2_PLACEMENT_3D('',#21641,#17784,#17785);
#14645=AXIS2_PLACEMENT_3D('',#21642,#17786,#17787);
#14646=AXIS2_PLACEMENT_3D('',#21644,#17788,#17789);
#14647=AXIS2_PLACEMENT_3D('',#21646,#17791,#17792);
#14648=AXIS2_PLACEMENT_3D('',#21647,#17793,#17794);
#14649=AXIS2_PLACEMENT_3D('',#21650,#17796,#17797);
#14650=AXIS2_PLACEMENT_3D('',#21651,#17798,#17799);
#14651=AXIS2_PLACEMENT_3D('',#21652,#17800,#17801);
#14652=AXIS2_PLACEMENT_3D('',#21653,#17802,#17803);
#14653=AXIS2_PLACEMENT_3D('',#21655,#17804,#17805);
#14654=AXIS2_PLACEMENT_3D('',#21658,#17807,#17808);
#14655=AXIS2_PLACEMENT_3D('',#21659,#17809,#17810);
#14656=AXIS2_PLACEMENT_3D('',#21661,#17811,#17812);
#14657=AXIS2_PLACEMENT_3D('',#21664,#17814,#17815);
#14658=AXIS2_PLACEMENT_3D('',#21665,#17816,#17817);
#14659=AXIS2_PLACEMENT_3D('',#21667,#17818,#17819);
#14660=AXIS2_PLACEMENT_3D('',#21670,#17821,#17822);
#14661=AXIS2_PLACEMENT_3D('',#21671,#17823,#17824);
#14662=AXIS2_PLACEMENT_3D('',#21673,#17825,#17826);
#14663=AXIS2_PLACEMENT_3D('',#21676,#17828,#17829);
#14664=AXIS2_PLACEMENT_3D('',#21677,#17830,#17831);
#14665=AXIS2_PLACEMENT_3D('',#21679,#17832,#17833);
#14666=AXIS2_PLACEMENT_3D('',#21682,#17835,#17836);
#14667=AXIS2_PLACEMENT_3D('',#21683,#17837,#17838);
#14668=AXIS2_PLACEMENT_3D('',#21685,#17839,#17840);
#14669=AXIS2_PLACEMENT_3D('',#21688,#17842,#17843);
#14670=AXIS2_PLACEMENT_3D('',#21689,#17844,#17845);
#14671=AXIS2_PLACEMENT_3D('',#21690,#17846,#17847);
#14672=AXIS2_PLACEMENT_3D('',#21691,#17848,#17849);
#14673=AXIS2_PLACEMENT_3D('',#21692,#17850,#17851);
#14674=AXIS2_PLACEMENT_3D('',#21694,#17852,#17853);
#14675=AXIS2_PLACEMENT_3D('',#21696,#17854,#17855);
#14676=AXIS2_PLACEMENT_3D('',#21697,#17856,#17857);
#14677=AXIS2_PLACEMENT_3D('',#21700,#17859,#17860);
#14678=AXIS2_PLACEMENT_3D('',#21701,#17861,#17862);
#14679=AXIS2_PLACEMENT_3D('',#21702,#17863,#17864);
#14680=AXIS2_PLACEMENT_3D('',#21704,#17865,#17866);
#14681=AXIS2_PLACEMENT_3D('',#21706,#17868,#17869);
#14682=AXIS2_PLACEMENT_3D('',#21707,#17870,#17871);
#14683=AXIS2_PLACEMENT_3D('',#21708,#17872,#17873);
#14684=AXIS2_PLACEMENT_3D('',#21710,#17874,#17875);
#14685=AXIS2_PLACEMENT_3D('',#21712,#17876,#17877);
#14686=AXIS2_PLACEMENT_3D('',#21713,#17878,#17879);
#14687=AXIS2_PLACEMENT_3D('',#21716,#17881,#17882);
#14688=AXIS2_PLACEMENT_3D('',#21717,#17883,#17884);
#14689=AXIS2_PLACEMENT_3D('',#21718,#17885,#17886);
#14690=AXIS2_PLACEMENT_3D('',#21720,#17887,#17888);
#14691=AXIS2_PLACEMENT_3D('',#21722,#17890,#17891);
#14692=AXIS2_PLACEMENT_3D('',#21723,#17892,#17893);
#14693=AXIS2_PLACEMENT_3D('',#21724,#17894,#17895);
#14694=AXIS2_PLACEMENT_3D('',#21726,#17896,#17897);
#14695=AXIS2_PLACEMENT_3D('',#21728,#17898,#17899);
#14696=AXIS2_PLACEMENT_3D('',#21729,#17900,#17901);
#14697=AXIS2_PLACEMENT_3D('',#21732,#17903,#17904);
#14698=AXIS2_PLACEMENT_3D('',#21733,#17905,#17906);
#14699=AXIS2_PLACEMENT_3D('',#21734,#17907,#17908);
#14700=AXIS2_PLACEMENT_3D('',#21736,#17909,#17910);
#14701=AXIS2_PLACEMENT_3D('',#21738,#17912,#17913);
#14702=AXIS2_PLACEMENT_3D('',#21739,#17914,#17915);
#14703=AXIS2_PLACEMENT_3D('',#21740,#17916,#17917);
#14704=AXIS2_PLACEMENT_3D('',#21742,#17918,#17919);
#14705=AXIS2_PLACEMENT_3D('',#21744,#17920,#17921);
#14706=AXIS2_PLACEMENT_3D('',#21745,#17922,#17923);
#14707=AXIS2_PLACEMENT_3D('',#21748,#17925,#17926);
#14708=AXIS2_PLACEMENT_3D('',#21749,#17927,#17928);
#14709=AXIS2_PLACEMENT_3D('',#21750,#17929,#17930);
#14710=AXIS2_PLACEMENT_3D('',#21752,#17931,#17932);
#14711=AXIS2_PLACEMENT_3D('',#21754,#17934,#17935);
#14712=AXIS2_PLACEMENT_3D('',#21755,#17936,#17937);
#14713=AXIS2_PLACEMENT_3D('',#21756,#17938,#17939);
#14714=AXIS2_PLACEMENT_3D('',#21758,#17940,#17941);
#14715=AXIS2_PLACEMENT_3D('',#21761,#17943,#17944);
#14716=AXIS2_PLACEMENT_3D('',#21762,#17945,#17946);
#14717=AXIS2_PLACEMENT_3D('',#21764,#17947,#17948);
#14718=AXIS2_PLACEMENT_3D('',#21767,#17950,#17951);
#14719=AXIS2_PLACEMENT_3D('',#21768,#17952,#17953);
#14720=AXIS2_PLACEMENT_3D('',#21770,#17954,#17955);
#14721=AXIS2_PLACEMENT_3D('',#21773,#17957,#17958);
#14722=AXIS2_PLACEMENT_3D('',#21774,#17959,#17960);
#14723=AXIS2_PLACEMENT_3D('',#21776,#17961,#17962);
#14724=AXIS2_PLACEMENT_3D('',#21779,#17964,#17965);
#14725=AXIS2_PLACEMENT_3D('',#21780,#17966,#17967);
#14726=AXIS2_PLACEMENT_3D('',#21782,#17968,#17969);
#14727=AXIS2_PLACEMENT_3D('',#21785,#17971,#17972);
#14728=AXIS2_PLACEMENT_3D('',#21786,#17973,#17974);
#14729=AXIS2_PLACEMENT_3D('',#21788,#17975,#17976);
#14730=AXIS2_PLACEMENT_3D('',#21791,#17978,#17979);
#14731=AXIS2_PLACEMENT_3D('',#21792,#17980,#17981);
#14732=AXIS2_PLACEMENT_3D('',#21793,#17982,#17983);
#14733=AXIS2_PLACEMENT_3D('',#21794,#17984,#17985);
#14734=AXIS2_PLACEMENT_3D('',#21795,#17986,#17987);
#14735=AXIS2_PLACEMENT_3D('',#21797,#17988,#17989);
#14736=AXIS2_PLACEMENT_3D('',#21799,#17990,#17991);
#14737=AXIS2_PLACEMENT_3D('',#21800,#17992,#17993);
#14738=AXIS2_PLACEMENT_3D('',#21802,#17994,#17995);
#14739=AXIS2_PLACEMENT_3D('',#21804,#17997,#17998);
#14740=AXIS2_PLACEMENT_3D('',#21805,#17999,#18000);
#14741=AXIS2_PLACEMENT_3D('',#21808,#18002,#18003);
#14742=AXIS2_PLACEMENT_3D('',#21809,#18004,#18005);
#14743=AXIS2_PLACEMENT_3D('',#21810,#18006,#18007);
#14744=AXIS2_PLACEMENT_3D('',#21811,#18008,#18009);
#14745=AXIS2_PLACEMENT_3D('',#21813,#18010,#18011);
#14746=AXIS2_PLACEMENT_3D('',#21815,#18012,#18013);
#14747=AXIS2_PLACEMENT_3D('',#21816,#18014,#18015);
#14748=AXIS2_PLACEMENT_3D('',#21818,#18016,#18017);
#14749=AXIS2_PLACEMENT_3D('',#21820,#18019,#18020);
#14750=AXIS2_PLACEMENT_3D('',#21821,#18021,#18022);
#14751=AXIS2_PLACEMENT_3D('',#21824,#18024,#18025);
#14752=AXIS2_PLACEMENT_3D('',#21825,#18026,#18027);
#14753=AXIS2_PLACEMENT_3D('',#21826,#18028,#18029);
#14754=AXIS2_PLACEMENT_3D('',#21827,#18030,#18031);
#14755=AXIS2_PLACEMENT_3D('',#21829,#18032,#18033);
#14756=AXIS2_PLACEMENT_3D('',#21831,#18034,#18035);
#14757=AXIS2_PLACEMENT_3D('',#21832,#18036,#18037);
#14758=AXIS2_PLACEMENT_3D('',#21834,#18038,#18039);
#14759=AXIS2_PLACEMENT_3D('',#21836,#18041,#18042);
#14760=AXIS2_PLACEMENT_3D('',#21837,#18043,#18044);
#14761=AXIS2_PLACEMENT_3D('',#21840,#18046,#18047);
#14762=AXIS2_PLACEMENT_3D('',#21841,#18048,#18049);
#14763=AXIS2_PLACEMENT_3D('',#21842,#18050,#18051);
#14764=AXIS2_PLACEMENT_3D('',#21843,#18052,#18053);
#14765=AXIS2_PLACEMENT_3D('',#21845,#18054,#18055);
#14766=AXIS2_PLACEMENT_3D('',#21847,#18056,#18057);
#14767=AXIS2_PLACEMENT_3D('',#21848,#18058,#18059);
#14768=AXIS2_PLACEMENT_3D('',#21850,#18060,#18061);
#14769=AXIS2_PLACEMENT_3D('',#21852,#18063,#18064);
#14770=AXIS2_PLACEMENT_3D('',#21853,#18065,#18066);
#14771=AXIS2_PLACEMENT_3D('',#21856,#18068,#18069);
#14772=AXIS2_PLACEMENT_3D('',#21857,#18070,#18071);
#14773=AXIS2_PLACEMENT_3D('',#21858,#18072,#18073);
#14774=AXIS2_PLACEMENT_3D('',#21859,#18074,#18075);
#14775=AXIS2_PLACEMENT_3D('',#21860,#18076,#18077);
#14776=AXIS2_PLACEMENT_3D('',#21863,#18078,#18079);
#14777=AXIS2_PLACEMENT_3D('',#21864,#18080,#18081);
#14778=AXIS2_PLACEMENT_3D('',#21866,#18082,#18083);
#14779=AXIS2_PLACEMENT_3D('',#21868,#18084,#18085);
#14780=AXIS2_PLACEMENT_3D('',#21869,#18086,#18087);
#14781=AXIS2_PLACEMENT_3D('',#21870,#18088,#18089);
#14782=AXIS2_PLACEMENT_3D('',#21873,#18091,#18092);
#14783=AXIS2_PLACEMENT_3D('',#21874,#18093,#18094);
#14784=AXIS2_PLACEMENT_3D('',#21876,#18095,#18096);
#14785=AXIS2_PLACEMENT_3D('',#21879,#18098,#18099);
#14786=AXIS2_PLACEMENT_3D('',#21880,#18100,#18101);
#14787=AXIS2_PLACEMENT_3D('',#21883,#18103,#18104);
#14788=AXIS2_PLACEMENT_3D('',#21884,#18105,#18106);
#14789=AXIS2_PLACEMENT_3D('',#21885,#18107,#18108);
#14790=AXIS2_PLACEMENT_3D('',#21887,#18109,#18110);
#14791=AXIS2_PLACEMENT_3D('',#21889,#18112,#18113);
#14792=AXIS2_PLACEMENT_3D('',#21891,#18114,#18115);
#14793=AXIS2_PLACEMENT_3D('',#21892,#18116,#18117);
#14794=AXIS2_PLACEMENT_3D('',#21894,#18119,#18120);
#14795=AXIS2_PLACEMENT_3D('',#21895,#18121,#18122);
#14796=AXIS2_PLACEMENT_3D('',#21898,#18123,#18124);
#14797=AXIS2_PLACEMENT_3D('',#21899,#18125,#18126);
#14798=AXIS2_PLACEMENT_3D('',#21901,#18127,#18128);
#14799=AXIS2_PLACEMENT_3D('',#21903,#18129,#18130);
#14800=AXIS2_PLACEMENT_3D('',#21904,#18131,#18132);
#14801=AXIS2_PLACEMENT_3D('',#21905,#18133,#18134);
#14802=AXIS2_PLACEMENT_3D('',#21907,#18135,#18136);
#14803=AXIS2_PLACEMENT_3D('',#21909,#18138,#18139);
#14804=AXIS2_PLACEMENT_3D('',#21911,#18140,#18141);
#14805=AXIS2_PLACEMENT_3D('',#21913,#18142,#18143);
#14806=AXIS2_PLACEMENT_3D('',#21914,#18144,#18145);
#14807=AXIS2_PLACEMENT_3D('',#21916,#18146,#18147);
#14808=AXIS2_PLACEMENT_3D('',#21918,#18149,#18150);
#14809=AXIS2_PLACEMENT_3D('',#21920,#18151,#18152);
#14810=AXIS2_PLACEMENT_3D('',#21922,#18154,#18155);
#14811=AXIS2_PLACEMENT_3D('',#21924,#18156,#18157);
#14812=AXIS2_PLACEMENT_3D('',#21926,#18159,#18160);
#14813=AXIS2_PLACEMENT_3D('',#21927,#18161,#18162);
#14814=AXIS2_PLACEMENT_3D('',#21929,#18164,#18165);
#14815=AXIS2_PLACEMENT_3D('',#21930,#18166,#18167);
#14816=AXIS2_PLACEMENT_3D('',#21933,#18168,#18169);
#14817=AXIS2_PLACEMENT_3D('',#21934,#18170,#18171);
#14818=AXIS2_PLACEMENT_3D('',#21937,#18172,#18173);
#14819=AXIS2_PLACEMENT_3D('',#21938,#18174,#18175);
#14820=AXIS2_PLACEMENT_3D('',#21941,#18176,#18177);
#14821=AXIS2_PLACEMENT_3D('',#21942,#18178,#18179);
#14822=AXIS2_PLACEMENT_3D('',#21945,#18180,#18181);
#14823=AXIS2_PLACEMENT_3D('',#21946,#18182,#18183);
#14824=AXIS2_PLACEMENT_3D('',#21949,#18184,#18185);
#14825=AXIS2_PLACEMENT_3D('',#21950,#18186,#18187);
#14826=AXIS2_PLACEMENT_3D('',#21953,#18188,#18189);
#14827=AXIS2_PLACEMENT_3D('',#21954,#18190,#18191);
#14828=AXIS2_PLACEMENT_3D('',#21957,#18192,#18193);
#14829=AXIS2_PLACEMENT_3D('',#21958,#18194,#18195);
#14830=AXIS2_PLACEMENT_3D('',#21959,#18196,#18197);
#14831=AXIS2_PLACEMENT_3D('',#21985,#18198,#18199);
#14832=AXIS2_PLACEMENT_3D('',#22009,#18200,#18201);
#14833=AXIS2_PLACEMENT_3D('',#22010,#18202,#18203);
#14834=AXIS2_PLACEMENT_3D('',#22012,#18204,#18205);
#14835=AXIS2_PLACEMENT_3D('',#22037,#18206,#18207);
#14836=AXIS2_PLACEMENT_3D('',#22062,#18208,#18209);
#14837=AXIS2_PLACEMENT_3D('',#22065,#18211,#18212);
#14838=AXIS2_PLACEMENT_3D('',#22067,#18213,#18214);
#14839=AXIS2_PLACEMENT_3D('',#22092,#18215,#18216);
#14840=AXIS2_PLACEMENT_3D('',#22117,#18217,#18218);
#14841=AXIS2_PLACEMENT_3D('',#22142,#18219,#18220);
#14842=AXIS2_PLACEMENT_3D('',#22166,#18221,#18222);
#14843=AXIS2_PLACEMENT_3D('',#22167,#18223,#18224);
#14844=AXIS2_PLACEMENT_3D('',#22169,#18225,#18226);
#14845=AXIS2_PLACEMENT_3D('',#22170,#18227,#18228);
#14846=AXIS2_PLACEMENT_3D('',#22171,#18229,#18230);
#14847=AXIS2_PLACEMENT_3D('',#22195,#18231,#18232);
#14848=AXIS2_PLACEMENT_3D('',#22196,#18233,#18234);
#14849=AXIS2_PLACEMENT_3D('',#22198,#18235,#18236);
#14850=AXIS2_PLACEMENT_3D('',#22199,#18237,#18238);
#14851=AXIS2_PLACEMENT_3D('',#22200,#18239,#18240);
#14852=AXIS2_PLACEMENT_3D('',#22224,#18241,#18242);
#14853=AXIS2_PLACEMENT_3D('',#22225,#18243,#18244);
#14854=AXIS2_PLACEMENT_3D('',#22227,#18245,#18246);
#14855=AXIS2_PLACEMENT_3D('',#22229,#18247,#18248);
#14856=AXIS2_PLACEMENT_3D('',#22230,#18249,#18250);
#14857=AXIS2_PLACEMENT_3D('',#22231,#18251,#18252);
#14858=AXIS2_PLACEMENT_3D('',#22255,#18253,#18254);
#14859=AXIS2_PLACEMENT_3D('',#22256,#18255,#18256);
#14860=AXIS2_PLACEMENT_3D('',#22258,#18257,#18258);
#14861=AXIS2_PLACEMENT_3D('',#22259,#18259,#18260);
#14862=AXIS2_PLACEMENT_3D('',#22260,#18261,#18262);
#14863=AXIS2_PLACEMENT_3D('',#22284,#18263,#18264);
#14864=AXIS2_PLACEMENT_3D('',#22285,#18265,#18266);
#14865=AXIS2_PLACEMENT_3D('',#22287,#18267,#18268);
#14866=AXIS2_PLACEMENT_3D('',#22288,#18269,#18270);
#14867=AXIS2_PLACEMENT_3D('',#22289,#18271,#18272);
#14868=AXIS2_PLACEMENT_3D('',#22313,#18273,#18274);
#14869=AXIS2_PLACEMENT_3D('',#22314,#18275,#18276);
#14870=AXIS2_PLACEMENT_3D('',#22316,#18277,#18278);
#14871=AXIS2_PLACEMENT_3D('',#22319,#18280,#18281);
#14872=AXIS2_PLACEMENT_3D('',#22343,#18282,#18283);
#14873=AXIS2_PLACEMENT_3D('',#22344,#18284,#18285);
#14874=AXIS2_PLACEMENT_3D('',#22345,#18286,#18287);
#14875=AXIS2_PLACEMENT_3D('',#22346,#18288,#18289);
#14876=AXIS2_PLACEMENT_3D('',#22347,#18290,#18291);
#14877=AXIS2_PLACEMENT_3D('',#22348,#18292,#18293);
#14878=AXIS2_PLACEMENT_3D('',#22349,#18294,#18295);
#14879=AXIS2_PLACEMENT_3D('',#22350,#18296,#18297);
#14880=AXIS2_PLACEMENT_3D('',#22351,#18298,#18299);
#14881=AXIS2_PLACEMENT_3D('',#22353,#18300,#18301);
#14882=AXIS2_PLACEMENT_3D('',#22355,#18302,#18303);
#14883=AXIS2_PLACEMENT_3D('',#22356,#18304,#18305);
#14884=AXIS2_PLACEMENT_3D('',#22358,#18306,#18307);
#14885=AXIS2_PLACEMENT_3D('',#22360,#18309,#18310);
#14886=AXIS2_PLACEMENT_3D('',#22362,#18311,#18312);
#14887=AXIS2_PLACEMENT_3D('',#22363,#18313,#18314);
#14888=AXIS2_PLACEMENT_3D('',#22365,#18316,#18317);
#14889=AXIS2_PLACEMENT_3D('',#22367,#18318,#18319);
#14890=AXIS2_PLACEMENT_3D('',#22369,#18320,#18321);
#14891=AXIS2_PLACEMENT_3D('',#22370,#18322,#18323);
#14892=AXIS2_PLACEMENT_3D('',#22372,#18324,#18325);
#14893=AXIS2_PLACEMENT_3D('',#22374,#18327,#18328);
#14894=AXIS2_PLACEMENT_3D('',#22376,#18329,#18330);
#14895=AXIS2_PLACEMENT_3D('',#22377,#18331,#18332);
#14896=AXIS2_PLACEMENT_3D('',#22379,#18334,#18335);
#14897=AXIS2_PLACEMENT_3D('',#22380,#18336,#18337);
#14898=AXIS2_PLACEMENT_3D('',#22381,#18338,#18339);
#14899=AXIS2_PLACEMENT_3D('',#22382,#18340,#18341);
#14900=AXIS2_PLACEMENT_3D('',#22383,#18342,#18343);
#14901=AXIS2_PLACEMENT_3D('',#22384,#18344,#18345);
#14902=AXIS2_PLACEMENT_3D('',#22385,#18346,#18347);
#14903=AXIS2_PLACEMENT_3D('',#22386,#18348,#18349);
#14904=AXIS2_PLACEMENT_3D('',#22387,#18350,#18351);
#14905=AXIS2_PLACEMENT_3D('',#22388,#18352,#18353);
#14906=AXIS2_PLACEMENT_3D('',#22389,#18354,#18355);
#14907=AXIS2_PLACEMENT_3D('',#22390,#18356,#18357);
#14908=AXIS2_PLACEMENT_3D('',#22391,#18358,#18359);
#14909=AXIS2_PLACEMENT_3D('',#22392,#18360,#18361);
#14910=AXIS2_PLACEMENT_3D('',#22393,#18362,#18363);
#14911=AXIS2_PLACEMENT_3D('',#22394,#18364,#18365);
#14912=AXIS2_PLACEMENT_3D('',#22395,#18366,#18367);
#14913=AXIS2_PLACEMENT_3D('',#22396,#18368,#18369);
#14914=AXIS2_PLACEMENT_3D('',#22397,#18370,#18371);
#14915=AXIS2_PLACEMENT_3D('',#22398,#18372,#18373);
#14916=AXIS2_PLACEMENT_3D('',#22399,#18374,#18375);
#14917=AXIS2_PLACEMENT_3D('',#22400,#18376,#18377);
#14918=AXIS2_PLACEMENT_3D('',#22401,#18378,#18379);
#14919=AXIS2_PLACEMENT_3D('',#22402,#18380,#18381);
#14920=AXIS2_PLACEMENT_3D('',#22403,#18382,#18383);
#14921=AXIS2_PLACEMENT_3D('',#22404,#18384,#18385);
#14922=AXIS2_PLACEMENT_3D('',#22405,#18386,#18387);
#14923=AXIS2_PLACEMENT_3D('',#22406,#18388,#18389);
#14924=AXIS2_PLACEMENT_3D('',#22407,#18390,#18391);
#14925=AXIS2_PLACEMENT_3D('',#22408,#18392,#18393);
#14926=AXIS2_PLACEMENT_3D('',#22409,#18394,#18395);
#14927=AXIS2_PLACEMENT_3D('',#22410,#18396,#18397);
#14928=AXIS2_PLACEMENT_3D('',#22411,#18398,#18399);
#14929=AXIS2_PLACEMENT_3D('',#22412,#18400,#18401);
#14930=AXIS2_PLACEMENT_3D('',#22413,#18402,#18403);
#14931=AXIS2_PLACEMENT_3D('',#22414,#18404,#18405);
#14932=AXIS2_PLACEMENT_3D('',#22415,#18406,#18407);
#14933=AXIS2_PLACEMENT_3D('',#22416,#18408,#18409);
#14934=AXIS2_PLACEMENT_3D('',#22417,#18410,#18411);
#14935=AXIS2_PLACEMENT_3D('',#22418,#18412,#18413);
#14936=AXIS2_PLACEMENT_3D('',#22419,#18414,#18415);
#14937=AXIS2_PLACEMENT_3D('',#22420,#18416,#18417);
#14938=AXIS2_PLACEMENT_3D('',#22421,#18418,#18419);
#14939=AXIS2_PLACEMENT_3D('',#22422,#18420,#18421);
#14940=AXIS2_PLACEMENT_3D('',#22423,#18422,#18423);
#14941=AXIS2_PLACEMENT_3D('',#22424,#18424,#18425);
#14942=AXIS2_PLACEMENT_3D('',#22425,#18426,#18427);
#14943=AXIS2_PLACEMENT_3D('',#22426,#18428,#18429);
#14944=AXIS2_PLACEMENT_3D('',#22427,#18430,#18431);
#14945=AXIS2_PLACEMENT_3D('',#22428,#18432,#18433);
#14946=AXIS2_PLACEMENT_3D('',#22429,#18434,#18435);
#14947=AXIS2_PLACEMENT_3D('',#22430,#18436,#18437);
#14948=AXIS2_PLACEMENT_3D('',#22431,#18438,#18439);
#14949=AXIS2_PLACEMENT_3D('',#22432,#18440,#18441);
#14950=AXIS2_PLACEMENT_3D('',#22434,#18442,#18443);
#14951=AXIS2_PLACEMENT_3D('',#22437,#18445,#18446);
#14952=AXIS2_PLACEMENT_3D('',#22438,#18447,#18448);
#14953=AXIS2_PLACEMENT_3D('',#22440,#18449,#18450);
#14954=AXIS2_PLACEMENT_3D('',#22443,#18452,#18453);
#14955=AXIS2_PLACEMENT_3D('',#22444,#18454,#18455);
#14956=AXIS2_PLACEMENT_3D('',#22446,#18456,#18457);
#14957=AXIS2_PLACEMENT_3D('',#22449,#18459,#18460);
#14958=AXIS2_PLACEMENT_3D('',#22450,#18461,#18462);
#14959=AXIS2_PLACEMENT_3D('',#22452,#18463,#18464);
#14960=AXIS2_PLACEMENT_3D('',#22455,#18466,#18467);
#14961=AXIS2_PLACEMENT_3D('',#22456,#18468,#18469);
#14962=AXIS2_PLACEMENT_3D('',#22458,#18470,#18471);
#14963=AXIS2_PLACEMENT_3D('',#22461,#18473,#18474);
#14964=AXIS2_PLACEMENT_3D('',#22462,#18475,#18476);
#14965=AXIS2_PLACEMENT_3D('',#22464,#18477,#18478);
#14966=AXIS2_PLACEMENT_3D('',#22467,#18480,#18481);
#14967=AXIS2_PLACEMENT_3D('',#22468,#18482,#18483);
#14968=AXIS2_PLACEMENT_3D('',#22470,#18484,#18485);
#14969=AXIS2_PLACEMENT_3D('',#22473,#18487,#18488);
#14970=AXIS2_PLACEMENT_3D('',#22474,#18489,#18490);
#14971=AXIS2_PLACEMENT_3D('',#22476,#18491,#18492);
#14972=AXIS2_PLACEMENT_3D('',#22479,#18494,#18495);
#14973=AXIS2_PLACEMENT_3D('',#22480,#18496,#18497);
#14974=AXIS2_PLACEMENT_3D('',#22489,#18502,#18503);
#14975=AXIS2_PLACEMENT_3D('',#22498,#18508,#18509);
#14976=AXIS2_PLACEMENT_3D('',#22501,#18512,#18513);
#14977=AXIS2_PLACEMENT_3D('',#22503,#18514,#18515);
#14978=AXIS2_PLACEMENT_3D('',#22506,#18517,#18518);
#14979=AXIS2_PLACEMENT_3D('',#22507,#18519,#18520);
#14980=AXIS2_PLACEMENT_3D('',#22509,#18521,#18522);
#14981=AXIS2_PLACEMENT_3D('',#22512,#18524,#18525);
#14982=AXIS2_PLACEMENT_3D('',#22513,#18526,#18527);
#14983=AXIS2_PLACEMENT_3D('',#22523,#18532,#18533);
#14984=AXIS2_PLACEMENT_3D('',#22525,#18535,#18536);
#14985=AXIS2_PLACEMENT_3D('',#22531,#18540,#18541);
#14986=AXIS2_PLACEMENT_3D('',#22537,#18545,#18546);
#14987=AXIS2_PLACEMENT_3D('',#22539,#18548,#18549);
#14988=AXIS2_PLACEMENT_3D('',#22541,#18551,#18552);
#14989=AXIS2_PLACEMENT_3D('',#22543,#18553,#18554);
#14990=AXIS2_PLACEMENT_3D('',#22545,#18556,#18557);
#14991=AXIS2_PLACEMENT_3D('',#22547,#18559,#18560);
#14992=AXIS2_PLACEMENT_3D('',#22548,#18561,#18562);
#14993=AXIS2_PLACEMENT_3D('',#22557,#18567,#18568);
#14994=AXIS2_PLACEMENT_3D('',#22563,#18572,#18573);
#14995=AXIS2_PLACEMENT_3D('',#22569,#18577,#18578);
#14996=AXIS2_PLACEMENT_3D('',#22572,#18581,#18582);
#14997=AXIS2_PLACEMENT_3D('',#22573,#18583,#18584);
#14998=AXIS2_PLACEMENT_3D('',#22574,#18585,#18586);
#14999=AXIS2_PLACEMENT_3D('',#22575,#18587,#18588);
#15000=AXIS2_PLACEMENT_3D('',#22584,#18593,#18594);
#15001=AXIS2_PLACEMENT_3D('',#22590,#18598,#18599);
#15002=AXIS2_PLACEMENT_3D('',#22596,#18603,#18604);
#15003=AXIS2_PLACEMENT_3D('',#22599,#18607,#18608);
#15004=AXIS2_PLACEMENT_3D('',#22600,#18609,#18610);
#15005=AXIS2_PLACEMENT_3D('',#22601,#18611,#18612);
#15006=AXIS2_PLACEMENT_3D('',#22602,#18613,#18614);
#15007=AXIS2_PLACEMENT_3D('',#22611,#18619,#18620);
#15008=AXIS2_PLACEMENT_3D('',#22617,#18624,#18625);
#15009=AXIS2_PLACEMENT_3D('',#22623,#18629,#18630);
#15010=AXIS2_PLACEMENT_3D('',#22626,#18633,#18634);
#15011=AXIS2_PLACEMENT_3D('',#22627,#18635,#18636);
#15012=AXIS2_PLACEMENT_3D('',#22628,#18637,#18638);
#15013=AXIS2_PLACEMENT_3D('',#22629,#18639,#18640);
#15014=AXIS2_PLACEMENT_3D('',#22631,#18641,#18642);
#15015=AXIS2_PLACEMENT_3D('',#22634,#18644,#18645);
#15016=AXIS2_PLACEMENT_3D('',#22635,#18646,#18647);
#15017=AXIS2_PLACEMENT_3D('',#22636,#18648,#18649);
#15018=AXIS2_PLACEMENT_3D('',#22638,#18650,#18651);
#15019=AXIS2_PLACEMENT_3D('',#22641,#18653,#18654);
#15020=AXIS2_PLACEMENT_3D('',#22642,#18655,#18656);
#15021=AXIS2_PLACEMENT_3D('',#22644,#18657,#18658);
#15022=AXIS2_PLACEMENT_3D('',#22647,#18660,#18661);
#15023=AXIS2_PLACEMENT_3D('',#22648,#18662,#18663);
#15024=AXIS2_PLACEMENT_3D('',#22650,#18664,#18665);
#15025=AXIS2_PLACEMENT_3D('',#22653,#18667,#18668);
#15026=AXIS2_PLACEMENT_3D('',#22654,#18669,#18670);
#15027=AXIS2_PLACEMENT_3D('',#22656,#18671,#18672);
#15028=AXIS2_PLACEMENT_3D('',#22658,#18673,#18674);
#15029=AXIS2_PLACEMENT_3D('',#22659,#18675,#18676);
#15030=AXIS2_PLACEMENT_3D('',#22661,#18677,#18678);
#15031=AXIS2_PLACEMENT_3D('',#22663,#18679,#18680);
#15032=AXIS2_PLACEMENT_3D('',#22664,#18681,#18682);
#15033=AXIS2_PLACEMENT_3D('',#22666,#18684,#18685);
#15034=AXIS2_PLACEMENT_3D('',#22669,#18687,#18688);
#15035=AXIS2_PLACEMENT_3D('',#22670,#18689,#18690);
#15036=AXIS2_PLACEMENT_3D('',#22672,#18691,#18692);
#15037=AXIS2_PLACEMENT_3D('',#22674,#18694,#18695);
#15038=AXIS2_PLACEMENT_3D('',#22675,#18696,#18697);
#15039=AXIS2_PLACEMENT_3D('',#22676,#18698,#18699);
#15040=AXIS2_PLACEMENT_3D('',#22677,#18700,#18701);
#15041=AXIS2_PLACEMENT_3D('',#22679,#18702,#18703);
#15042=AXIS2_PLACEMENT_3D('',#22682,#18705,#18706);
#15043=AXIS2_PLACEMENT_3D('',#22683,#18707,#18708);
#15044=AXIS2_PLACEMENT_3D('',#22685,#18709,#18710);
#15045=AXIS2_PLACEMENT_3D('',#22688,#18712,#18713);
#15046=AXIS2_PLACEMENT_3D('',#22689,#18714,#18715);
#15047=AXIS2_PLACEMENT_3D('',#22690,#18716,#18717);
#15048=AXIS2_PLACEMENT_3D('',#22691,#18718,#18719);
#15049=AXIS2_PLACEMENT_3D('',#22692,#18720,#18721);
#15050=AXIS2_PLACEMENT_3D('',#22694,#18722,#18723);
#15051=AXIS2_PLACEMENT_3D('',#22697,#18725,#18726);
#15052=AXIS2_PLACEMENT_3D('',#22698,#18727,#18728);
#15053=AXIS2_PLACEMENT_3D('',#22700,#18729,#18730);
#15054=AXIS2_PLACEMENT_3D('',#22703,#18732,#18733);
#15055=AXIS2_PLACEMENT_3D('',#22704,#18734,#18735);
#15056=AXIS2_PLACEMENT_3D('',#22705,#18736,#18737);
#15057=AXIS2_PLACEMENT_3D('',#22706,#18738,#18739);
#15058=AXIS2_PLACEMENT_3D('',#22707,#18740,#18741);
#15059=AXIS2_PLACEMENT_3D('',#22709,#18742,#18743);
#15060=AXIS2_PLACEMENT_3D('',#22712,#18745,#18746);
#15061=AXIS2_PLACEMENT_3D('',#22713,#18747,#18748);
#15062=AXIS2_PLACEMENT_3D('',#22715,#18749,#18750);
#15063=AXIS2_PLACEMENT_3D('',#22718,#18752,#18753);
#15064=AXIS2_PLACEMENT_3D('',#22719,#18754,#18755);
#15065=AXIS2_PLACEMENT_3D('',#22720,#18756,#18757);
#15066=AXIS2_PLACEMENT_3D('',#22721,#18758,#18759);
#15067=AXIS2_PLACEMENT_3D('',#22722,#18760,#18761);
#15068=AXIS2_PLACEMENT_3D('',#22724,#18762,#18763);
#15069=AXIS2_PLACEMENT_3D('',#22727,#18765,#18766);
#15070=AXIS2_PLACEMENT_3D('',#22728,#18767,#18768);
#15071=AXIS2_PLACEMENT_3D('',#22730,#18769,#18770);
#15072=AXIS2_PLACEMENT_3D('',#22733,#18772,#18773);
#15073=AXIS2_PLACEMENT_3D('',#22734,#18774,#18775);
#15074=AXIS2_PLACEMENT_3D('',#22735,#18776,#18777);
#15075=AXIS2_PLACEMENT_3D('',#22736,#18778,#18779);
#15076=AXIS2_PLACEMENT_3D('',#22737,#18780,#18781);
#15077=AXIS2_PLACEMENT_3D('',#22739,#18782,#18783);
#15078=AXIS2_PLACEMENT_3D('',#22742,#18785,#18786);
#15079=AXIS2_PLACEMENT_3D('',#22743,#18787,#18788);
#15080=AXIS2_PLACEMENT_3D('',#22744,#18789,#18790);
#15081=AXIS2_PLACEMENT_3D('',#22746,#18791,#18792);
#15082=AXIS2_PLACEMENT_3D('',#22749,#18794,#18795);
#15083=AXIS2_PLACEMENT_3D('',#22750,#18796,#18797);
#15084=AXIS2_PLACEMENT_3D('',#22752,#18798,#18799);
#15085=AXIS2_PLACEMENT_3D('',#22755,#18801,#18802);
#15086=AXIS2_PLACEMENT_3D('',#22756,#18803,#18804);
#15087=AXIS2_PLACEMENT_3D('',#22758,#18805,#18806);
#15088=AXIS2_PLACEMENT_3D('',#22761,#18808,#18809);
#15089=AXIS2_PLACEMENT_3D('',#22762,#18810,#18811);
#15090=AXIS2_PLACEMENT_3D('',#22764,#18812,#18813);
#15091=AXIS2_PLACEMENT_3D('',#22766,#18814,#18815);
#15092=AXIS2_PLACEMENT_3D('',#22767,#18816,#18817);
#15093=AXIS2_PLACEMENT_3D('',#22769,#18818,#18819);
#15094=AXIS2_PLACEMENT_3D('',#22771,#18820,#18821);
#15095=AXIS2_PLACEMENT_3D('',#22772,#18822,#18823);
#15096=AXIS2_PLACEMENT_3D('',#22774,#18825,#18826);
#15097=AXIS2_PLACEMENT_3D('',#22777,#18828,#18829);
#15098=AXIS2_PLACEMENT_3D('',#22778,#18830,#18831);
#15099=AXIS2_PLACEMENT_3D('',#22780,#18832,#18833);
#15100=AXIS2_PLACEMENT_3D('',#22782,#18835,#18836);
#15101=AXIS2_PLACEMENT_3D('',#22783,#18837,#18838);
#15102=AXIS2_PLACEMENT_3D('',#22784,#18839,#18840);
#15103=AXIS2_PLACEMENT_3D('',#22785,#18841,#18842);
#15104=AXIS2_PLACEMENT_3D('',#22787,#18843,#18844);
#15105=AXIS2_PLACEMENT_3D('',#22790,#18846,#18847);
#15106=AXIS2_PLACEMENT_3D('',#22791,#18848,#18849);
#15107=AXIS2_PLACEMENT_3D('',#22793,#18850,#18851);
#15108=AXIS2_PLACEMENT_3D('',#22796,#18853,#18854);
#15109=AXIS2_PLACEMENT_3D('',#22797,#18855,#18856);
#15110=AXIS2_PLACEMENT_3D('',#22798,#18857,#18858);
#15111=AXIS2_PLACEMENT_3D('',#22799,#18859,#18860);
#15112=AXIS2_PLACEMENT_3D('',#22800,#18861,#18862);
#15113=AXIS2_PLACEMENT_3D('',#22802,#18863,#18864);
#15114=AXIS2_PLACEMENT_3D('',#22805,#18866,#18867);
#15115=AXIS2_PLACEMENT_3D('',#22806,#18868,#18869);
#15116=AXIS2_PLACEMENT_3D('',#22808,#18870,#18871);
#15117=AXIS2_PLACEMENT_3D('',#22811,#18873,#18874);
#15118=AXIS2_PLACEMENT_3D('',#22812,#18875,#18876);
#15119=AXIS2_PLACEMENT_3D('',#22813,#18877,#18878);
#15120=AXIS2_PLACEMENT_3D('',#22814,#18879,#18880);
#15121=AXIS2_PLACEMENT_3D('',#22815,#18881,#18882);
#15122=AXIS2_PLACEMENT_3D('',#22817,#18883,#18884);
#15123=AXIS2_PLACEMENT_3D('',#22820,#18886,#18887);
#15124=AXIS2_PLACEMENT_3D('',#22821,#18888,#18889);
#15125=AXIS2_PLACEMENT_3D('',#22823,#18890,#18891);
#15126=AXIS2_PLACEMENT_3D('',#22826,#18893,#18894);
#15127=AXIS2_PLACEMENT_3D('',#22827,#18895,#18896);
#15128=AXIS2_PLACEMENT_3D('',#22828,#18897,#18898);
#15129=AXIS2_PLACEMENT_3D('',#22829,#18899,#18900);
#15130=AXIS2_PLACEMENT_3D('',#22830,#18901,#18902);
#15131=AXIS2_PLACEMENT_3D('',#22832,#18903,#18904);
#15132=AXIS2_PLACEMENT_3D('',#22833,#18905,#18906);
#15133=AXIS2_PLACEMENT_3D('',#22835,#18907,#18908);
#15134=AXIS2_PLACEMENT_3D('',#22837,#18910,#18911);
#15135=AXIS2_PLACEMENT_3D('',#22839,#18912,#18913);
#15136=AXIS2_PLACEMENT_3D('',#22841,#18915,#18916);
#15137=AXIS2_PLACEMENT_3D('',#22843,#18917,#18918);
#15138=AXIS2_PLACEMENT_3D('',#22845,#18920,#18921);
#15139=AXIS2_PLACEMENT_3D('',#22847,#18922,#18923);
#15140=AXIS2_PLACEMENT_3D('',#22848,#18924,#18925);
#15141=AXIS2_PLACEMENT_3D('',#22850,#18926,#18927);
#15142=AXIS2_PLACEMENT_3D('',#22852,#18929,#18930);
#15143=AXIS2_PLACEMENT_3D('',#22854,#18931,#18932);
#15144=AXIS2_PLACEMENT_3D('',#22856,#18934,#18935);
#15145=AXIS2_PLACEMENT_3D('',#22858,#18936,#18937);
#15146=AXIS2_PLACEMENT_3D('',#22860,#18939,#18940);
#15147=AXIS2_PLACEMENT_3D('',#22861,#18941,#18942);
#15148=AXIS2_PLACEMENT_3D('',#22870,#18947,#18948);
#15149=AXIS2_PLACEMENT_3D('',#22876,#18952,#18953);
#15150=AXIS2_PLACEMENT_3D('',#22882,#18957,#18958);
#15151=AXIS2_PLACEMENT_3D('',#22888,#18962,#18963);
#15152=AXIS2_PLACEMENT_3D('',#22894,#18967,#18968);
#15153=AXIS2_PLACEMENT_3D('',#22897,#18971,#18972);
#15154=AXIS2_PLACEMENT_3D('',#22898,#18973,#18974);
#15155=AXIS2_PLACEMENT_3D('',#22899,#18975,#18976);
#15156=AXIS2_PLACEMENT_3D('',#22900,#18977,#18978);
#15157=AXIS2_PLACEMENT_3D('',#22901,#18979,#18980);
#15158=AXIS2_PLACEMENT_3D('',#22902,#18981,#18982);
#15159=AXIS2_PLACEMENT_3D('',#22903,#18983,#18984);
#15160=AXIS2_PLACEMENT_3D('',#22904,#18985,#18986);
#15161=AXIS2_PLACEMENT_3D('',#22905,#18987,#18988);
#15162=AXIS2_PLACEMENT_3D('',#22906,#18989,#18990);
#15163=AXIS2_PLACEMENT_3D('',#22907,#18991,#18992);
#15164=AXIS2_PLACEMENT_3D('',#22908,#18993,#18994);
#15165=AXIS2_PLACEMENT_3D('',#22909,#18995,#18996);
#15166=AXIS2_PLACEMENT_3D('',#22910,#18997,#18998);
#15167=AXIS2_PLACEMENT_3D('',#22911,#18999,#19000);
#15168=AXIS2_PLACEMENT_3D('',#22912,#19001,#19002);
#15169=AXIS2_PLACEMENT_3D('',#22913,#19003,#19004);
#15170=AXIS2_PLACEMENT_3D('',#22914,#19005,#19006);
#15171=AXIS2_PLACEMENT_3D('',#22915,#19007,#19008);
#15172=AXIS2_PLACEMENT_3D('',#22916,#19009,#19010);
#15173=AXIS2_PLACEMENT_3D('',#22917,#19011,#19012);
#15174=AXIS2_PLACEMENT_3D('',#22918,#19013,#19014);
#15175=AXIS2_PLACEMENT_3D('',#22919,#19015,#19016);
#15176=AXIS2_PLACEMENT_3D('',#22920,#19017,#19018);
#15177=AXIS2_PLACEMENT_3D('',#22921,#19019,#19020);
#15178=AXIS2_PLACEMENT_3D('',#22922,#19021,#19022);
#15179=AXIS2_PLACEMENT_3D('',#22923,#19023,#19024);
#15180=AXIS2_PLACEMENT_3D('',#22924,#19025,#19026);
#15181=AXIS2_PLACEMENT_3D('',#22925,#19027,#19028);
#15182=AXIS2_PLACEMENT_3D('',#22926,#19029,#19030);
#15183=AXIS2_PLACEMENT_3D('',#22927,#19031,#19032);
#15184=AXIS2_PLACEMENT_3D('',#22928,#19033,#19034);
#15185=AXIS2_PLACEMENT_3D('',#22929,#19035,#19036);
#15186=AXIS2_PLACEMENT_3D('',#22930,#19037,#19038);
#15187=AXIS2_PLACEMENT_3D('',#22931,#19039,#19040);
#15188=AXIS2_PLACEMENT_3D('',#22932,#19041,#19042);
#15189=AXIS2_PLACEMENT_3D('',#22933,#19043,#19044);
#15190=AXIS2_PLACEMENT_3D('',#22934,#19045,#19046);
#15191=AXIS2_PLACEMENT_3D('',#22935,#19047,#19048);
#15192=AXIS2_PLACEMENT_3D('',#22936,#19049,#19050);
#15193=AXIS2_PLACEMENT_3D('',#22937,#19051,#19052);
#15194=AXIS2_PLACEMENT_3D('',#22938,#19053,#19054);
#15195=AXIS2_PLACEMENT_3D('',#22939,#19055,#19056);
#15196=AXIS2_PLACEMENT_3D('',#22940,#19057,#19058);
#15197=AXIS2_PLACEMENT_3D('',#22941,#19059,#19060);
#15198=AXIS2_PLACEMENT_3D('',#22942,#19061,#19062);
#15199=AXIS2_PLACEMENT_3D('',#22943,#19063,#19064);
#15200=AXIS2_PLACEMENT_3D('',#22944,#19065,#19066);
#15201=AXIS2_PLACEMENT_3D('',#22945,#19067,#19068);
#15202=AXIS2_PLACEMENT_3D('',#22946,#19069,#19070);
#15203=AXIS2_PLACEMENT_3D('',#22947,#19071,#19072);
#15204=AXIS2_PLACEMENT_3D('',#22948,#19073,#19074);
#15205=AXIS2_PLACEMENT_3D('',#22949,#19075,#19076);
#15206=AXIS2_PLACEMENT_3D('',#22950,#19077,#19078);
#15207=AXIS2_PLACEMENT_3D('',#22951,#19079,#19080);
#15208=AXIS2_PLACEMENT_3D('',#22952,#19081,#19082);
#15209=AXIS2_PLACEMENT_3D('',#22953,#19083,#19084);
#15210=AXIS2_PLACEMENT_3D('',#22954,#19085,#19086);
#15211=AXIS2_PLACEMENT_3D('',#22955,#19087,#19088);
#15212=AXIS2_PLACEMENT_3D('',#22956,#19089,#19090);
#15213=AXIS2_PLACEMENT_3D('',#22957,#19091,#19092);
#15214=AXIS2_PLACEMENT_3D('',#22958,#19093,#19094);
#15215=AXIS2_PLACEMENT_3D('',#22959,#19095,#19096);
#15216=AXIS2_PLACEMENT_3D('',#22960,#19097,#19098);
#15217=AXIS2_PLACEMENT_3D('',#22961,#19099,#19100);
#15218=AXIS2_PLACEMENT_3D('',#22962,#19101,#19102);
#15219=AXIS2_PLACEMENT_3D('',#22963,#19103,#19104);
#15220=AXIS2_PLACEMENT_3D('',#22964,#19105,#19106);
#15221=AXIS2_PLACEMENT_3D('',#22965,#19107,#19108);
#15222=AXIS2_PLACEMENT_3D('',#22966,#19109,#19110);
#15223=AXIS2_PLACEMENT_3D('',#22967,#19111,#19112);
#15224=AXIS2_PLACEMENT_3D('',#22968,#19113,#19114);
#15225=AXIS2_PLACEMENT_3D('',#22969,#19115,#19116);
#15226=AXIS2_PLACEMENT_3D('',#22970,#19117,#19118);
#15227=AXIS2_PLACEMENT_3D('',#22971,#19119,#19120);
#15228=AXIS2_PLACEMENT_3D('',#22972,#19121,#19122);
#15229=AXIS2_PLACEMENT_3D('',#22974,#19123,#19124);
#15230=AXIS2_PLACEMENT_3D('',#22977,#19126,#19127);
#15231=AXIS2_PLACEMENT_3D('',#22978,#19128,#19129);
#15232=AXIS2_PLACEMENT_3D('',#22980,#19130,#19131);
#15233=AXIS2_PLACEMENT_3D('',#22983,#19133,#19134);
#15234=AXIS2_PLACEMENT_3D('',#22984,#19135,#19136);
#15235=AXIS2_PLACEMENT_3D('',#22986,#19137,#19138);
#15236=AXIS2_PLACEMENT_3D('',#22989,#19140,#19141);
#15237=AXIS2_PLACEMENT_3D('',#22990,#19142,#19143);
#15238=AXIS2_PLACEMENT_3D('',#22999,#19148,#19149);
#15239=AXIS2_PLACEMENT_3D('',#23005,#19153,#19154);
#15240=AXIS2_PLACEMENT_3D('',#23011,#19158,#19159);
#15241=AXIS2_PLACEMENT_3D('',#23014,#19162,#19163);
#15242=AXIS2_PLACEMENT_3D('',#23015,#19164,#19165);
#15243=AXIS2_PLACEMENT_3D('',#23016,#19166,#19167);
#15244=AXIS2_PLACEMENT_3D('',#23017,#19168,#19169);
#15245=AXIS2_PLACEMENT_3D('',#23019,#19170,#19171);
#15246=AXIS2_PLACEMENT_3D('',#23022,#19173,#19174);
#15247=AXIS2_PLACEMENT_3D('',#23023,#19175,#19176);
#15248=AXIS2_PLACEMENT_3D('',#23025,#19177,#19178);
#15249=AXIS2_PLACEMENT_3D('',#23028,#19180,#19181);
#15250=AXIS2_PLACEMENT_3D('',#23029,#19182,#19183);
#15251=AXIS2_PLACEMENT_3D('',#23031,#19184,#19185);
#15252=AXIS2_PLACEMENT_3D('',#23034,#19187,#19188);
#15253=AXIS2_PLACEMENT_3D('',#23035,#19189,#19190);
#15254=AXIS2_PLACEMENT_3D('',#23044,#19195,#19196);
#15255=AXIS2_PLACEMENT_3D('',#23050,#19200,#19201);
#15256=AXIS2_PLACEMENT_3D('',#23056,#19205,#19206);
#15257=AXIS2_PLACEMENT_3D('',#23059,#19209,#19210);
#15258=AXIS2_PLACEMENT_3D('',#23060,#19211,#19212);
#15259=AXIS2_PLACEMENT_3D('',#23061,#19213,#19214);
#15260=AXIS2_PLACEMENT_3D('',#23062,#19215,#19216);
#15261=AXIS2_PLACEMENT_3D('',#23064,#19217,#19218);
#15262=AXIS2_PLACEMENT_3D('',#23067,#19220,#19221);
#15263=AXIS2_PLACEMENT_3D('',#23068,#19222,#19223);
#15264=AXIS2_PLACEMENT_3D('',#23070,#19224,#19225);
#15265=AXIS2_PLACEMENT_3D('',#23073,#19227,#19228);
#15266=AXIS2_PLACEMENT_3D('',#23074,#19229,#19230);
#15267=AXIS2_PLACEMENT_3D('',#23076,#19231,#19232);
#15268=AXIS2_PLACEMENT_3D('',#23079,#19234,#19235);
#15269=AXIS2_PLACEMENT_3D('',#23080,#19236,#19237);
#15270=AXIS2_PLACEMENT_3D('',#23089,#19242,#19243);
#15271=AXIS2_PLACEMENT_3D('',#23095,#19247,#19248);
#15272=AXIS2_PLACEMENT_3D('',#23101,#19252,#19253);
#15273=AXIS2_PLACEMENT_3D('',#23104,#19256,#19257);
#15274=AXIS2_PLACEMENT_3D('',#23105,#19258,#19259);
#15275=AXIS2_PLACEMENT_3D('',#23106,#19260,#19261);
#15276=AXIS2_PLACEMENT_3D('',#23107,#19262,#19263);
#15277=AXIS2_PLACEMENT_3D('',#23109,#19264,#19265);
#15278=AXIS2_PLACEMENT_3D('',#23112,#19267,#19268);
#15279=AXIS2_PLACEMENT_3D('',#23113,#19269,#19270);
#15280=AXIS2_PLACEMENT_3D('',#23122,#19275,#19276);
#15281=AXIS2_PLACEMENT_3D('',#23128,#19280,#19281);
#15282=AXIS2_PLACEMENT_3D('',#23134,#19285,#19286);
#15283=AXIS2_PLACEMENT_3D('',#23137,#19289,#19290);
#15284=AXIS2_PLACEMENT_3D('',#23138,#19291,#19292);
#15285=AXIS2_PLACEMENT_3D('',#23139,#19293,#19294);
#15286=AXIS2_PLACEMENT_3D('',#23140,#19295,#19296);
#15287=AXIS2_PLACEMENT_3D('',#23142,#19297,#19298);
#15288=AXIS2_PLACEMENT_3D('',#23145,#19300,#19301);
#15289=AXIS2_PLACEMENT_3D('',#23146,#19302,#19303);
#15290=AXIS2_PLACEMENT_3D('',#23147,#19304,#19305);
#15291=AXIS2_PLACEMENT_3D('',#23149,#19306,#19307);
#15292=AXIS2_PLACEMENT_3D('',#23151,#19308,#19309);
#15293=AXIS2_PLACEMENT_3D('',#23152,#19310,#19311);
#15294=AXIS2_PLACEMENT_3D('',#23155,#19313,#19314);
#15295=AXIS2_PLACEMENT_3D('',#23156,#19315,#19316);
#15296=AXIS2_PLACEMENT_3D('',#23157,#19317,#19318);
#15297=AXIS2_PLACEMENT_3D('',#23159,#19319,#19320);
#15298=AXIS2_PLACEMENT_3D('',#23161,#19322,#19323);
#15299=AXIS2_PLACEMENT_3D('',#23162,#19324,#19325);
#15300=AXIS2_PLACEMENT_3D('',#23163,#19326,#19327);
#15301=AXIS2_PLACEMENT_3D('',#23165,#19328,#19329);
#15302=AXIS2_PLACEMENT_3D('',#23168,#19331,#19332);
#15303=AXIS2_PLACEMENT_3D('',#23169,#19333,#19334);
#15304=AXIS2_PLACEMENT_3D('',#23171,#19335,#19336);
#15305=AXIS2_PLACEMENT_3D('',#23174,#19338,#19339);
#15306=AXIS2_PLACEMENT_3D('',#23175,#19340,#19341);
#15307=AXIS2_PLACEMENT_3D('',#23176,#19342,#19343);
#15308=AXIS2_PLACEMENT_3D('',#23177,#19344,#19345);
#15309=AXIS2_PLACEMENT_3D('',#23178,#19346,#19347);
#15310=AXIS2_PLACEMENT_3D('',#23180,#19348,#19349);
#15311=AXIS2_PLACEMENT_3D('',#23183,#19351,#19352);
#15312=AXIS2_PLACEMENT_3D('',#23184,#19353,#19354);
#15313=AXIS2_PLACEMENT_3D('',#23186,#19355,#19356);
#15314=AXIS2_PLACEMENT_3D('',#23189,#19358,#19359);
#15315=AXIS2_PLACEMENT_3D('',#23190,#19360,#19361);
#15316=AXIS2_PLACEMENT_3D('',#23191,#19362,#19363);
#15317=AXIS2_PLACEMENT_3D('',#23192,#19364,#19365);
#15318=AXIS2_PLACEMENT_3D('',#23193,#19366,#19367);
#15319=AXIS2_PLACEMENT_3D('',#23194,#19368,#19369);
#15320=AXIS2_PLACEMENT_3D('',#23197,#19370,#19371);
#15321=AXIS2_PLACEMENT_3D('',#23203,#19375,#19376);
#15322=AXIS2_PLACEMENT_3D('',#23209,#19380,#19381);
#15323=AXIS2_PLACEMENT_3D('',#23211,#19382,#19383);
#15324=AXIS2_PLACEMENT_3D('',#23215,#19386,#19387);
#15325=AXIS2_PLACEMENT_3D('',#23218,#19390,#19391);
#15326=AXIS2_PLACEMENT_3D('',#23219,#19392,#19393);
#15327=AXIS2_PLACEMENT_3D('',#23221,#19394,#19395);
#15328=AXIS2_PLACEMENT_3D('',#23223,#19396,#19397);
#15329=AXIS2_PLACEMENT_3D('',#23224,#19398,#19399);
#15330=AXIS2_PLACEMENT_3D('',#23226,#19400,#19401);
#15331=AXIS2_PLACEMENT_3D('',#23228,#19403,#19404);
#15332=AXIS2_PLACEMENT_3D('',#23230,#19405,#19406);
#15333=AXIS2_PLACEMENT_3D('',#23231,#19407,#19408);
#15334=AXIS2_PLACEMENT_3D('',#23233,#19409,#19410);
#15335=AXIS2_PLACEMENT_3D('',#23235,#19412,#19413);
#15336=AXIS2_PLACEMENT_3D('',#23237,#19414,#19415);
#15337=AXIS2_PLACEMENT_3D('',#23238,#19416,#19417);
#15338=AXIS2_PLACEMENT_3D('',#23240,#19418,#19419);
#15339=AXIS2_PLACEMENT_3D('',#23242,#19421,#19422);
#15340=AXIS2_PLACEMENT_3D('',#23244,#19423,#19424);
#15341=AXIS2_PLACEMENT_3D('',#23245,#19425,#19426);
#15342=AXIS2_PLACEMENT_3D('',#23247,#19427,#19428);
#15343=AXIS2_PLACEMENT_3D('',#23249,#19430,#19431);
#15344=AXIS2_PLACEMENT_3D('',#23251,#19432,#19433);
#15345=AXIS2_PLACEMENT_3D('',#23252,#19434,#19435);
#15346=AXIS2_PLACEMENT_3D('',#23254,#19436,#19437);
#15347=AXIS2_PLACEMENT_3D('',#23256,#19439,#19440);
#15348=AXIS2_PLACEMENT_3D('',#23258,#19441,#19442);
#15349=AXIS2_PLACEMENT_3D('',#23259,#19443,#19444);
#15350=AXIS2_PLACEMENT_3D('',#23261,#19446,#19447);
#15351=AXIS2_PLACEMENT_3D('',#23262,#19448,#19449);
#15352=AXIS2_PLACEMENT_3D('',#23265,#19450,#19451);
#15353=AXIS2_PLACEMENT_3D('',#23269,#19453,#19454);
#15354=AXIS2_PLACEMENT_3D('',#23271,#19456,#19457);
#15355=AXIS2_PLACEMENT_3D('',#23277,#19461,#19462);
#15356=AXIS2_PLACEMENT_3D('',#23279,#19463,#19464);
#15357=AXIS2_PLACEMENT_3D('',#23281,#19465,#19466);
#15358=AXIS2_PLACEMENT_3D('',#23283,#19468,#19469);
#15359=AXIS2_PLACEMENT_3D('',#23286,#19472,#19473);
#15360=AXIS2_PLACEMENT_3D('',#23288,#19474,#19475);
#15361=AXIS2_PLACEMENT_3D('',#23290,#19476,#19477);
#15362=AXIS2_PLACEMENT_3D('',#23291,#19478,#19479);
#15363=AXIS2_PLACEMENT_3D('',#23293,#19480,#19481);
#15364=AXIS2_PLACEMENT_3D('',#23295,#19483,#19484);
#15365=AXIS2_PLACEMENT_3D('',#23297,#19485,#19486);
#15366=AXIS2_PLACEMENT_3D('',#23298,#19487,#19488);
#15367=AXIS2_PLACEMENT_3D('',#23300,#19490,#19491);
#15368=AXIS2_PLACEMENT_3D('',#23301,#19492,#19493);
#15369=AXIS2_PLACEMENT_3D('',#23302,#19494,#19495);
#15370=AXIS2_PLACEMENT_3D('',#23303,#19496,#19497);
#15371=AXIS2_PLACEMENT_3D('',#23312,#19502,#19503);
#15372=AXIS2_PLACEMENT_3D('',#23318,#19507,#19508);
#15373=AXIS2_PLACEMENT_3D('',#23324,#19512,#19513);
#15374=AXIS2_PLACEMENT_3D('',#23330,#19517,#19518);
#15375=AXIS2_PLACEMENT_3D('',#23336,#19522,#19523);
#15376=AXIS2_PLACEMENT_3D('',#23339,#19526,#19527);
#15377=AXIS2_PLACEMENT_3D('',#23340,#19528,#19529);
#15378=AXIS2_PLACEMENT_3D('',#23341,#19530,#19531);
#15379=AXIS2_PLACEMENT_3D('',#23343,#19532,#19533);
#15380=AXIS2_PLACEMENT_3D('',#23344,#19534,#19535);
#15381=AXIS2_PLACEMENT_3D('',#23346,#19536,#19537);
#15382=AXIS2_PLACEMENT_3D('',#23347,#19538,#19539);
#15383=AXIS2_PLACEMENT_3D('',#23349,#19540,#19541);
#15384=AXIS2_PLACEMENT_3D('',#23351,#19543,#19544);
#15385=AXIS2_PLACEMENT_3D('',#23353,#19545,#19546);
#15386=AXIS2_PLACEMENT_3D('',#23355,#19548,#19549);
#15387=AXIS2_PLACEMENT_3D('',#23357,#19550,#19551);
#15388=AXIS2_PLACEMENT_3D('',#23359,#19553,#19554);
#15389=AXIS2_PLACEMENT_3D('',#23361,#19555,#19556);
#15390=AXIS2_PLACEMENT_3D('',#23362,#19557,#19558);
#15391=AXIS2_PLACEMENT_3D('',#23364,#19559,#19560);
#15392=AXIS2_PLACEMENT_3D('',#23366,#19562,#19563);
#15393=AXIS2_PLACEMENT_3D('',#23368,#19565,#19566);
#15394=AXIS2_PLACEMENT_3D('',#23369,#19567,#19568);
#15395=AXIS2_PLACEMENT_3D('',#23370,#19569,#19570);
#15396=AXIS2_PLACEMENT_3D('',#23371,#19571,#19572);
#15397=AXIS2_PLACEMENT_3D('',#23372,#19573,#19574);
#15398=AXIS2_PLACEMENT_3D('',#23373,#19575,#19576);
#15399=AXIS2_PLACEMENT_3D('',#23374,#19577,#19578);
#15400=AXIS2_PLACEMENT_3D('',#23375,#19579,#19580);
#15401=AXIS2_PLACEMENT_3D('',#23376,#19581,#19582);
#15402=AXIS2_PLACEMENT_3D('',#23377,#19583,#19584);
#15403=AXIS2_PLACEMENT_3D('',#23378,#19585,#19586);
#15404=AXIS2_PLACEMENT_3D('',#23379,#19587,#19588);
#15405=AXIS2_PLACEMENT_3D('',#23380,#19589,#19590);
#15406=AXIS2_PLACEMENT_3D('',#23382,#19591,#19592);
#15407=AXIS2_PLACEMENT_3D('',#23385,#19594,#19595);
#15408=AXIS2_PLACEMENT_3D('',#23386,#19596,#19597);
#15409=AXIS2_PLACEMENT_3D('',#23391,#19599,#19600);
#15410=AXIS2_PLACEMENT_3D('',#23394,#19602,#19603);
#15411=AXIS2_PLACEMENT_3D('',#23395,#19604,#19605);
#15412=AXIS2_PLACEMENT_3D('',#23399,#19607,#19608);
#15413=AXIS2_PLACEMENT_3D('',#23402,#19610,#19611);
#15414=AXIS2_PLACEMENT_3D('',#23403,#19612,#19613);
#15415=AXIS2_PLACEMENT_3D('',#23407,#19616,#19617);
#15416=AXIS2_PLACEMENT_3D('',#23410,#19619,#19620);
#15417=AXIS2_PLACEMENT_3D('',#23411,#19621,#19622);
#15418=AXIS2_PLACEMENT_3D('',#23414,#19624,#19625);
#15419=AXIS2_PLACEMENT_3D('',#23415,#19626,#19627);
#15420=AXIS2_PLACEMENT_3D('',#23417,#19629,#19630);
#15421=AXIS2_PLACEMENT_3D('',#23418,#19631,#19632);
#15422=AXIS2_PLACEMENT_3D('',#23419,#19633,#19634);
#15423=AXIS2_PLACEMENT_3D('',#23420,#19635,#19636);
#15424=AXIS2_PLACEMENT_3D('',#23421,#19637,#19638);
#15425=AXIS2_PLACEMENT_3D('',#23423,#19639,#19640);
#15426=AXIS2_PLACEMENT_3D('',#23426,#19642,#19643);
#15427=AXIS2_PLACEMENT_3D('',#23427,#19644,#19645);
#15428=AXIS2_PLACEMENT_3D('',#23428,#19646,#19647);
#15429=AXIS2_PLACEMENT_3D('',#23429,#19648,#19649);
#15430=AXIS2_PLACEMENT_3D('',#23430,#19650,#19651);
#15431=AXIS2_PLACEMENT_3D('',#23432,#19652,#19653);
#15432=AXIS2_PLACEMENT_3D('',#23435,#19655,#19656);
#15433=AXIS2_PLACEMENT_3D('',#23436,#19657,#19658);
#15434=AXIS2_PLACEMENT_3D('',#23438,#19659,#19660);
#15435=AXIS2_PLACEMENT_3D('',#23441,#19662,#19663);
#15436=AXIS2_PLACEMENT_3D('',#23442,#19664,#19665);
#15437=AXIS2_PLACEMENT_3D('',#23443,#19666,#19667);
#15438=AXIS2_PLACEMENT_3D('',#23444,#19668,#19669);
#15439=AXIS2_PLACEMENT_3D('',#23445,#19670,#19671);
#15440=AXIS2_PLACEMENT_3D('',#23447,#19672,#19673);
#15441=AXIS2_PLACEMENT_3D('',#23450,#19675,#19676);
#15442=AXIS2_PLACEMENT_3D('',#23451,#19677,#19678);
#15443=AXIS2_PLACEMENT_3D('',#23453,#19679,#19680);
#15444=AXIS2_PLACEMENT_3D('',#23456,#19682,#19683);
#15445=AXIS2_PLACEMENT_3D('',#23457,#19684,#19685);
#15446=AXIS2_PLACEMENT_3D('',#23458,#19686,#19687);
#15447=AXIS2_PLACEMENT_3D('',#23459,#19688,#19689);
#15448=AXIS2_PLACEMENT_3D('',#23460,#19690,#19691);
#15449=AXIS2_PLACEMENT_3D('',#23462,#19692,#19693);
#15450=AXIS2_PLACEMENT_3D('',#23465,#19695,#19696);
#15451=AXIS2_PLACEMENT_3D('',#23466,#19697,#19698);
#15452=AXIS2_PLACEMENT_3D('',#23468,#19699,#19700);
#15453=AXIS2_PLACEMENT_3D('',#23471,#19702,#19703);
#15454=AXIS2_PLACEMENT_3D('',#23472,#19704,#19705);
#15455=AXIS2_PLACEMENT_3D('',#23473,#19706,#19707);
#15456=AXIS2_PLACEMENT_3D('',#23474,#19708,#19709);
#15457=AXIS2_PLACEMENT_3D('',#23475,#19710,#19711);
#15458=AXIS2_PLACEMENT_3D('',#23477,#19712,#19713);
#15459=AXIS2_PLACEMENT_3D('',#23480,#19715,#19716);
#15460=AXIS2_PLACEMENT_3D('',#23481,#19717,#19718);
#15461=AXIS2_PLACEMENT_3D('',#23482,#19719,#19720);
#15462=AXIS2_PLACEMENT_3D('',#23483,#19721,#19722);
#15463=AXIS2_PLACEMENT_3D('',#23484,#19723,#19724);
#15464=AXIS2_PLACEMENT_3D('',#23485,#19725,#19726);
#15465=AXIS2_PLACEMENT_3D('',#23486,#19727,#19728);
#15466=AXIS2_PLACEMENT_3D('',#23487,#19729,#19730);
#15467=AXIS2_PLACEMENT_3D('',#23488,#19731,#19732);
#15468=AXIS2_PLACEMENT_3D('',#23489,#19733,#19734);
#15469=AXIS2_PLACEMENT_3D('',#23490,#19735,#19736);
#15470=AXIS2_PLACEMENT_3D('',#23491,#19737,#19738);
#15471=AXIS2_PLACEMENT_3D('',#23492,#19739,#19740);
#15472=AXIS2_PLACEMENT_3D('',#23493,#19741,#19742);
#15473=AXIS2_PLACEMENT_3D('',#23494,#19743,#19744);
#15474=DIRECTION('axis',(0.,0.,1.));
#15475=DIRECTION('refdir',(1.,0.,0.));
#15476=DIRECTION('axis',(0.,0.,1.));
#15477=DIRECTION('refdir',(1.,0.,0.));
#15478=DIRECTION('axis',(0.,0.,1.));
#15479=DIRECTION('refdir',(1.,0.,0.));
#15480=DIRECTION('center_axis',(0.,0.,1.));
#15481=DIRECTION('ref_axis',(1.,0.,0.));
#15482=DIRECTION('center_axis',(0.,0.,1.));
#15483=DIRECTION('ref_axis',(1.,0.,0.));
#15484=DIRECTION('',(0.,0.,1.));
#15485=DIRECTION('center_axis',(0.,0.,-1.));
#15486=DIRECTION('ref_axis',(1.,0.,0.));
#15487=DIRECTION('center_axis',(0.,0.,1.));
#15488=DIRECTION('ref_axis',(1.,0.,0.));
#15489=DIRECTION('center_axis',(0.,0.,1.));
#15490=DIRECTION('ref_axis',(1.,0.,0.));
#15491=DIRECTION('',(0.,0.,1.));
#15492=DIRECTION('center_axis',(0.,0.,-1.));
#15493=DIRECTION('ref_axis',(1.,0.,0.));
#15494=DIRECTION('center_axis',(0.,0.,1.));
#15495=DIRECTION('ref_axis',(1.,0.,0.));
#15496=DIRECTION('center_axis',(0.,0.,1.));
#15497=DIRECTION('ref_axis',(1.,0.,0.));
#15498=DIRECTION('',(0.,0.,1.));
#15499=DIRECTION('center_axis',(0.,0.,-1.));
#15500=DIRECTION('ref_axis',(1.,0.,0.));
#15501=DIRECTION('center_axis',(0.,0.,1.));
#15502=DIRECTION('ref_axis',(1.,0.,0.));
#15503=DIRECTION('center_axis',(0.,0.,1.));
#15504=DIRECTION('ref_axis',(1.,0.,0.));
#15505=DIRECTION('',(0.,0.,1.));
#15506=DIRECTION('center_axis',(0.,0.,-1.));
#15507=DIRECTION('ref_axis',(1.,0.,0.));
#15508=DIRECTION('center_axis',(0.,0.,1.));
#15509=DIRECTION('ref_axis',(1.,0.,0.));
#15510=DIRECTION('center_axis',(0.,0.,1.));
#15511=DIRECTION('ref_axis',(1.,0.,0.));
#15512=DIRECTION('',(0.,0.,1.));
#15513=DIRECTION('center_axis',(0.,0.,-1.));
#15514=DIRECTION('ref_axis',(1.,0.,0.));
#15515=DIRECTION('center_axis',(0.,0.,1.));
#15516=DIRECTION('ref_axis',(1.,0.,0.));
#15517=DIRECTION('center_axis',(0.,0.,1.));
#15518=DIRECTION('ref_axis',(1.,0.,0.));
#15519=DIRECTION('',(0.,0.,1.));
#15520=DIRECTION('center_axis',(0.,0.,-1.));
#15521=DIRECTION('ref_axis',(1.,0.,0.));
#15522=DIRECTION('center_axis',(0.,0.,1.));
#15523=DIRECTION('ref_axis',(1.,0.,0.));
#15524=DIRECTION('center_axis',(0.,0.,1.));
#15525=DIRECTION('ref_axis',(1.,0.,0.));
#15526=DIRECTION('',(0.,0.,1.));
#15527=DIRECTION('center_axis',(0.,0.,-1.));
#15528=DIRECTION('ref_axis',(1.,0.,0.));
#15529=DIRECTION('center_axis',(0.,0.,1.));
#15530=DIRECTION('ref_axis',(1.,0.,0.));
#15531=DIRECTION('center_axis',(0.,0.,1.));
#15532=DIRECTION('ref_axis',(1.,0.,0.));
#15533=DIRECTION('',(0.,0.,1.));
#15534=DIRECTION('center_axis',(0.,0.,-1.));
#15535=DIRECTION('ref_axis',(1.,0.,0.));
#15536=DIRECTION('center_axis',(0.,0.,1.));
#15537=DIRECTION('ref_axis',(1.,0.,0.));
#15538=DIRECTION('center_axis',(0.,0.,1.));
#15539=DIRECTION('ref_axis',(1.,0.,0.));
#15540=DIRECTION('',(0.,0.,1.));
#15541=DIRECTION('center_axis',(0.,0.,-1.));
#15542=DIRECTION('ref_axis',(1.,0.,0.));
#15543=DIRECTION('center_axis',(0.,0.,1.));
#15544=DIRECTION('ref_axis',(1.,0.,0.));
#15545=DIRECTION('center_axis',(0.,0.,1.));
#15546=DIRECTION('ref_axis',(1.,0.,0.));
#15547=DIRECTION('',(0.,0.,1.));
#15548=DIRECTION('center_axis',(0.,0.,-1.));
#15549=DIRECTION('ref_axis',(1.,0.,0.));
#15550=DIRECTION('center_axis',(0.,0.,1.));
#15551=DIRECTION('ref_axis',(1.,0.,0.));
#15552=DIRECTION('center_axis',(0.,0.,1.));
#15553=DIRECTION('ref_axis',(1.,0.,0.));
#15554=DIRECTION('',(0.,0.,1.));
#15555=DIRECTION('center_axis',(0.,0.,-1.));
#15556=DIRECTION('ref_axis',(1.,0.,0.));
#15557=DIRECTION('center_axis',(0.,0.,1.));
#15558=DIRECTION('ref_axis',(1.,0.,0.));
#15559=DIRECTION('center_axis',(0.,0.,1.));
#15560=DIRECTION('ref_axis',(1.,0.,0.));
#15561=DIRECTION('',(0.,0.,1.));
#15562=DIRECTION('center_axis',(0.,0.,-1.));
#15563=DIRECTION('ref_axis',(1.,0.,0.));
#15564=DIRECTION('center_axis',(0.,1.,0.));
#15565=DIRECTION('ref_axis',(-1.,0.,0.));
#15566=DIRECTION('',(-1.,0.,0.));
#15567=DIRECTION('',(0.,0.,1.));
#15568=DIRECTION('',(-1.,0.,0.));
#15569=DIRECTION('',(0.,0.,1.));
#15570=DIRECTION('center_axis',(1.,0.,0.));
#15571=DIRECTION('ref_axis',(0.,1.,0.));
#15572=DIRECTION('',(0.,1.,0.));
#15573=DIRECTION('',(0.,1.,0.));
#15574=DIRECTION('',(0.,0.,1.));
#15575=DIRECTION('center_axis',(0.,-1.,0.));
#15576=DIRECTION('ref_axis',(1.,0.,0.));
#15577=DIRECTION('',(1.,0.,0.));
#15578=DIRECTION('',(1.,0.,0.));
#15579=DIRECTION('',(0.,0.,1.));
#15580=DIRECTION('center_axis',(-1.,0.,0.));
#15581=DIRECTION('ref_axis',(0.,-1.,0.));
#15582=DIRECTION('',(0.,-1.,0.));
#15583=DIRECTION('',(0.,-1.,0.));
#15584=DIRECTION('center_axis',(0.,0.,1.));
#15585=DIRECTION('ref_axis',(1.,0.,0.));
#15586=DIRECTION('center_axis',(0.,0.,1.));
#15587=DIRECTION('ref_axis',(1.,0.,0.));
#15588=DIRECTION('axis',(0.,0.,1.));
#15589=DIRECTION('refdir',(1.,0.,0.));
#15590=DIRECTION('center_axis',(0.,1.,0.));
#15591=DIRECTION('ref_axis',(-1.,0.,0.));
#15592=DIRECTION('',(-1.,0.,0.));
#15593=DIRECTION('',(0.,0.,1.));
#15594=DIRECTION('',(-1.,0.,0.));
#15595=DIRECTION('',(0.,0.,1.));
#15596=DIRECTION('center_axis',(1.,0.,0.));
#15597=DIRECTION('ref_axis',(0.,1.,0.));
#15598=DIRECTION('',(0.,1.,0.));
#15599=DIRECTION('',(0.,1.,0.));
#15600=DIRECTION('',(0.,0.,1.));
#15601=DIRECTION('center_axis',(0.,-1.,0.));
#15602=DIRECTION('ref_axis',(1.,0.,0.));
#15603=DIRECTION('',(1.,0.,0.));
#15604=DIRECTION('',(1.,0.,0.));
#15605=DIRECTION('',(0.,0.,1.));
#15606=DIRECTION('center_axis',(-1.,0.,0.));
#15607=DIRECTION('ref_axis',(0.,-1.,0.));
#15608=DIRECTION('',(0.,-1.,0.));
#15609=DIRECTION('',(0.,-1.,0.));
#15610=DIRECTION('center_axis',(0.,0.,1.));
#15611=DIRECTION('ref_axis',(1.,0.,0.));
#15612=DIRECTION('center_axis',(0.,0.,1.));
#15613=DIRECTION('ref_axis',(1.,0.,0.));
#15614=DIRECTION('axis',(0.,0.,1.));
#15615=DIRECTION('refdir',(1.,0.,0.));
#15616=DIRECTION('center_axis',(0.,1.,0.));
#15617=DIRECTION('ref_axis',(-1.,0.,0.));
#15618=DIRECTION('',(-1.,0.,0.));
#15619=DIRECTION('',(0.,0.,1.));
#15620=DIRECTION('',(-1.,0.,0.));
#15621=DIRECTION('',(0.,0.,1.));
#15622=DIRECTION('center_axis',(1.,0.,0.));
#15623=DIRECTION('ref_axis',(0.,1.,0.));
#15624=DIRECTION('',(0.,1.,0.));
#15625=DIRECTION('',(0.,1.,0.));
#15626=DIRECTION('',(0.,0.,1.));
#15627=DIRECTION('center_axis',(0.,-1.,0.));
#15628=DIRECTION('ref_axis',(1.,0.,0.));
#15629=DIRECTION('',(1.,0.,0.));
#15630=DIRECTION('',(1.,0.,0.));
#15631=DIRECTION('',(0.,0.,1.));
#15632=DIRECTION('center_axis',(-1.,0.,0.));
#15633=DIRECTION('ref_axis',(0.,-1.,0.));
#15634=DIRECTION('',(0.,-1.,0.));
#15635=DIRECTION('',(0.,-1.,0.));
#15636=DIRECTION('center_axis',(0.,0.,1.));
#15637=DIRECTION('ref_axis',(1.,0.,0.));
#15638=DIRECTION('center_axis',(0.,0.,1.));
#15639=DIRECTION('ref_axis',(1.,0.,0.));
#15640=DIRECTION('axis',(0.,0.,1.));
#15641=DIRECTION('refdir',(1.,0.,0.));
#15642=DIRECTION('center_axis',(0.,1.,0.));
#15643=DIRECTION('ref_axis',(1.,0.,0.));
#15644=DIRECTION('center_axis',(0.,1.,0.));
#15645=DIRECTION('ref_axis',(1.,0.,0.));
#15646=DIRECTION('',(0.,1.,0.));
#15647=DIRECTION('center_axis',(0.,-1.,0.));
#15648=DIRECTION('ref_axis',(1.,0.,0.));
#15649=DIRECTION('center_axis',(0.,1.,0.));
#15650=DIRECTION('ref_axis',(1.,0.,0.));
#15651=DIRECTION('center_axis',(0.,1.,0.));
#15652=DIRECTION('ref_axis',(1.,0.,0.));
#15653=DIRECTION('',(0.,1.,0.));
#15654=DIRECTION('center_axis',(0.,-1.,0.));
#15655=DIRECTION('ref_axis',(1.,0.,0.));
#15656=DIRECTION('center_axis',(0.,1.,0.));
#15657=DIRECTION('ref_axis',(1.,0.,0.));
#15658=DIRECTION('center_axis',(0.,1.,0.));
#15659=DIRECTION('ref_axis',(1.,0.,0.));
#15660=DIRECTION('',(0.,1.,0.));
#15661=DIRECTION('center_axis',(0.,-1.,0.));
#15662=DIRECTION('ref_axis',(1.,0.,0.));
#15663=DIRECTION('center_axis',(0.,1.,0.));
#15664=DIRECTION('ref_axis',(1.,0.,0.));
#15665=DIRECTION('center_axis',(0.,1.,0.));
#15666=DIRECTION('ref_axis',(1.,0.,0.));
#15667=DIRECTION('',(0.,1.,0.));
#15668=DIRECTION('center_axis',(0.,-1.,0.));
#15669=DIRECTION('ref_axis',(1.,0.,0.));
#15670=DIRECTION('center_axis',(0.,0.,1.));
#15671=DIRECTION('ref_axis',(1.,0.,0.));
#15672=DIRECTION('center_axis',(0.,0.,1.));
#15673=DIRECTION('ref_axis',(1.,0.,0.));
#15674=DIRECTION('',(0.,0.,1.));
#15675=DIRECTION('center_axis',(0.,0.,-1.));
#15676=DIRECTION('ref_axis',(1.,0.,0.));
#15677=DIRECTION('center_axis',(0.,0.,1.));
#15678=DIRECTION('ref_axis',(1.,0.,0.));
#15679=DIRECTION('center_axis',(0.,0.,1.));
#15680=DIRECTION('ref_axis',(1.,0.,0.));
#15681=DIRECTION('',(0.,0.,1.));
#15682=DIRECTION('center_axis',(0.,0.,-1.));
#15683=DIRECTION('ref_axis',(1.,0.,0.));
#15684=DIRECTION('center_axis',(0.,0.,1.));
#15685=DIRECTION('ref_axis',(1.,0.,0.));
#15686=DIRECTION('center_axis',(0.,0.,1.));
#15687=DIRECTION('ref_axis',(1.,0.,0.));
#15688=DIRECTION('',(0.,0.,1.));
#15689=DIRECTION('center_axis',(0.,0.,-1.));
#15690=DIRECTION('ref_axis',(1.,0.,0.));
#15691=DIRECTION('center_axis',(0.,0.,1.));
#15692=DIRECTION('ref_axis',(1.,0.,0.));
#15693=DIRECTION('center_axis',(0.,0.,1.));
#15694=DIRECTION('ref_axis',(1.,0.,0.));
#15695=DIRECTION('',(0.,0.,1.));
#15696=DIRECTION('center_axis',(0.,0.,-1.));
#15697=DIRECTION('ref_axis',(1.,0.,0.));
#15698=DIRECTION('center_axis',(0.,0.,1.));
#15699=DIRECTION('ref_axis',(1.,0.,0.));
#15700=DIRECTION('',(0.,-1.,0.));
#15701=DIRECTION('',(-1.,0.,0.));
#15702=DIRECTION('',(0.,1.,0.));
#15703=DIRECTION('',(-1.,0.,0.));
#15704=DIRECTION('',(0.,1.,0.));
#15705=DIRECTION('',(1.,0.,0.));
#15706=DIRECTION('',(0.,1.,0.));
#15707=DIRECTION('',(-1.,0.,0.));
#15708=DIRECTION('center_axis',(-1.,0.,0.));
#15709=DIRECTION('ref_axis',(0.,0.,1.));
#15710=DIRECTION('',(0.,0.,-1.));
#15711=DIRECTION('',(0.,0.,1.));
#15712=DIRECTION('',(0.,1.,0.));
#15713=DIRECTION('center_axis',(1.,0.,0.));
#15714=DIRECTION('ref_axis',(0.,0.,-1.));
#15715=DIRECTION('',(0.,0.,1.));
#15716=DIRECTION('',(0.,1.,0.));
#15717=DIRECTION('',(0.,0.,-1.));
#15718=DIRECTION('center_axis',(0.,1.,0.));
#15719=DIRECTION('ref_axis',(0.,0.,1.));
#15720=DIRECTION('',(-1.,0.,0.));
#15721=DIRECTION('center_axis',(0.,-1.,0.));
#15722=DIRECTION('ref_axis',(1.,0.,0.));
#15723=DIRECTION('',(0.,0.,1.));
#15724=DIRECTION('',(1.,0.,0.));
#15725=DIRECTION('',(0.,0.,1.));
#15726=DIRECTION('',(1.,0.,0.));
#15727=DIRECTION('center_axis',(1.,0.,0.));
#15728=DIRECTION('ref_axis',(0.,1.,0.));
#15729=DIRECTION('',(0.,0.,1.));
#15730=DIRECTION('',(0.,1.,0.));
#15731=DIRECTION('center_axis',(0.,1.,0.));
#15732=DIRECTION('ref_axis',(-1.,0.,0.));
#15733=DIRECTION('',(0.,0.,1.));
#15734=DIRECTION('',(-1.,0.,0.));
#15735=DIRECTION('center_axis',(-1.,0.,0.));
#15736=DIRECTION('ref_axis',(0.,-1.,0.));
#15737=DIRECTION('',(0.,-1.,0.));
#15738=DIRECTION('center_axis',(0.,0.,1.));
#15739=DIRECTION('ref_axis',(1.,0.,0.));
#15740=DIRECTION('center_axis',(0.,0.,1.));
#15741=DIRECTION('ref_axis',(1.,0.,0.));
#15742=DIRECTION('axis',(0.,0.,1.));
#15743=DIRECTION('refdir',(1.,0.,0.));
#15744=DIRECTION('center_axis',(0.,1.,0.));
#15745=DIRECTION('ref_axis',(1.,0.,0.));
#15746=DIRECTION('center_axis',(0.,1.,0.));
#15747=DIRECTION('ref_axis',(1.,0.,0.));
#15748=DIRECTION('',(0.,1.,0.));
#15749=DIRECTION('center_axis',(0.,-1.,0.));
#15750=DIRECTION('ref_axis',(1.,0.,0.));
#15751=DIRECTION('center_axis',(0.,1.,0.));
#15752=DIRECTION('ref_axis',(1.,0.,0.));
#15753=DIRECTION('center_axis',(0.,1.,0.));
#15754=DIRECTION('ref_axis',(1.,0.,0.));
#15755=DIRECTION('',(0.,1.,0.));
#15756=DIRECTION('center_axis',(0.,-1.,0.));
#15757=DIRECTION('ref_axis',(1.,0.,0.));
#15758=DIRECTION('center_axis',(0.,1.,0.));
#15759=DIRECTION('ref_axis',(1.,0.,0.));
#15760=DIRECTION('center_axis',(0.,1.,0.));
#15761=DIRECTION('ref_axis',(1.,0.,0.));
#15762=DIRECTION('',(0.,1.,0.));
#15763=DIRECTION('center_axis',(0.,-1.,0.));
#15764=DIRECTION('ref_axis',(1.,0.,0.));
#15765=DIRECTION('center_axis',(0.,1.,0.));
#15766=DIRECTION('ref_axis',(1.,0.,0.));
#15767=DIRECTION('center_axis',(0.,1.,0.));
#15768=DIRECTION('ref_axis',(1.,0.,0.));
#15769=DIRECTION('',(0.,1.,0.));
#15770=DIRECTION('center_axis',(0.,-1.,0.));
#15771=DIRECTION('ref_axis',(1.,0.,0.));
#15772=DIRECTION('center_axis',(0.,0.,1.));
#15773=DIRECTION('ref_axis',(1.,0.,0.));
#15774=DIRECTION('center_axis',(0.,0.,1.));
#15775=DIRECTION('ref_axis',(1.,0.,0.));
#15776=DIRECTION('',(0.,0.,1.));
#15777=DIRECTION('center_axis',(0.,0.,-1.));
#15778=DIRECTION('ref_axis',(1.,0.,0.));
#15779=DIRECTION('center_axis',(0.,0.,1.));
#15780=DIRECTION('ref_axis',(1.,0.,0.));
#15781=DIRECTION('center_axis',(0.,0.,1.));
#15782=DIRECTION('ref_axis',(1.,0.,0.));
#15783=DIRECTION('',(0.,0.,1.));
#15784=DIRECTION('center_axis',(0.,0.,-1.));
#15785=DIRECTION('ref_axis',(1.,0.,0.));
#15786=DIRECTION('center_axis',(0.,0.,1.));
#15787=DIRECTION('ref_axis',(1.,0.,0.));
#15788=DIRECTION('center_axis',(0.,0.,1.));
#15789=DIRECTION('ref_axis',(1.,0.,0.));
#15790=DIRECTION('',(0.,0.,1.));
#15791=DIRECTION('center_axis',(0.,0.,-1.));
#15792=DIRECTION('ref_axis',(1.,0.,0.));
#15793=DIRECTION('center_axis',(0.,0.,1.));
#15794=DIRECTION('ref_axis',(1.,0.,0.));
#15795=DIRECTION('center_axis',(0.,0.,1.));
#15796=DIRECTION('ref_axis',(1.,0.,0.));
#15797=DIRECTION('',(0.,0.,1.));
#15798=DIRECTION('center_axis',(0.,0.,-1.));
#15799=DIRECTION('ref_axis',(1.,0.,0.));
#15800=DIRECTION('center_axis',(0.,0.,1.));
#15801=DIRECTION('ref_axis',(1.,0.,0.));
#15802=DIRECTION('',(0.,-1.,0.));
#15803=DIRECTION('',(-1.,0.,0.));
#15804=DIRECTION('',(0.,1.,0.));
#15805=DIRECTION('',(-1.,0.,0.));
#15806=DIRECTION('',(0.,1.,0.));
#15807=DIRECTION('',(1.,0.,0.));
#15808=DIRECTION('',(0.,1.,0.));
#15809=DIRECTION('',(-1.,0.,0.));
#15810=DIRECTION('center_axis',(-1.,0.,0.));
#15811=DIRECTION('ref_axis',(0.,0.,1.));
#15812=DIRECTION('',(0.,0.,-1.));
#15813=DIRECTION('',(0.,0.,1.));
#15814=DIRECTION('',(0.,1.,0.));
#15815=DIRECTION('center_axis',(1.,0.,0.));
#15816=DIRECTION('ref_axis',(0.,0.,-1.));
#15817=DIRECTION('',(0.,0.,1.));
#15818=DIRECTION('',(0.,1.,0.));
#15819=DIRECTION('',(0.,0.,-1.));
#15820=DIRECTION('center_axis',(0.,1.,0.));
#15821=DIRECTION('ref_axis',(0.,0.,1.));
#15822=DIRECTION('',(-1.,0.,0.));
#15823=DIRECTION('center_axis',(0.,-1.,0.));
#15824=DIRECTION('ref_axis',(1.,0.,0.));
#15825=DIRECTION('',(0.,0.,1.));
#15826=DIRECTION('',(1.,0.,0.));
#15827=DIRECTION('',(0.,0.,1.));
#15828=DIRECTION('',(1.,0.,0.));
#15829=DIRECTION('center_axis',(1.,0.,0.));
#15830=DIRECTION('ref_axis',(0.,1.,0.));
#15831=DIRECTION('',(0.,0.,1.));
#15832=DIRECTION('',(0.,1.,0.));
#15833=DIRECTION('center_axis',(0.,1.,0.));
#15834=DIRECTION('ref_axis',(-1.,0.,0.));
#15835=DIRECTION('',(0.,0.,1.));
#15836=DIRECTION('',(-1.,0.,0.));
#15837=DIRECTION('center_axis',(-1.,0.,0.));
#15838=DIRECTION('ref_axis',(0.,-1.,0.));
#15839=DIRECTION('',(0.,-1.,0.));
#15840=DIRECTION('center_axis',(0.,0.,1.));
#15841=DIRECTION('ref_axis',(1.,0.,0.));
#15842=DIRECTION('center_axis',(0.,0.,1.));
#15843=DIRECTION('ref_axis',(1.,0.,0.));
#15844=DIRECTION('axis',(0.,0.,1.));
#15845=DIRECTION('refdir',(1.,0.,0.));
#15846=DIRECTION('center_axis',(0.,1.,0.));
#15847=DIRECTION('ref_axis',(1.,0.,0.));
#15848=DIRECTION('center_axis',(0.,1.,0.));
#15849=DIRECTION('ref_axis',(1.,0.,0.));
#15850=DIRECTION('',(0.,1.,0.));
#15851=DIRECTION('center_axis',(0.,1.,0.));
#15852=DIRECTION('ref_axis',(1.,0.,0.));
#15853=DIRECTION('center_axis',(0.,1.,0.));
#15854=DIRECTION('ref_axis',(1.,0.,0.));
#15855=DIRECTION('center_axis',(0.,1.,0.));
#15856=DIRECTION('ref_axis',(1.,0.,0.));
#15857=DIRECTION('center_axis',(0.,1.,0.));
#15858=DIRECTION('ref_axis',(1.,0.,0.));
#15859=DIRECTION('',(0.,1.,0.));
#15860=DIRECTION('center_axis',(0.,-1.,0.));
#15861=DIRECTION('ref_axis',(1.,0.,0.));
#15862=DIRECTION('center_axis',(0.,1.,0.));
#15863=DIRECTION('ref_axis',(1.,0.,0.));
#15864=DIRECTION('center_axis',(0.,1.,0.));
#15865=DIRECTION('ref_axis',(1.,0.,0.));
#15866=DIRECTION('',(0.,1.,0.));
#15867=DIRECTION('center_axis',(0.,-1.,0.));
#15868=DIRECTION('ref_axis',(1.,0.,0.));
#15869=DIRECTION('center_axis',(0.,1.,0.));
#15870=DIRECTION('ref_axis',(1.,0.,0.));
#15871=DIRECTION('center_axis',(0.,1.,0.));
#15872=DIRECTION('ref_axis',(1.,0.,0.));
#15873=DIRECTION('',(0.,1.,0.));
#15874=DIRECTION('center_axis',(0.,-1.,0.));
#15875=DIRECTION('ref_axis',(1.,0.,0.));
#15876=DIRECTION('center_axis',(0.,1.,0.));
#15877=DIRECTION('ref_axis',(1.,0.,0.));
#15878=DIRECTION('center_axis',(0.,1.,0.));
#15879=DIRECTION('ref_axis',(1.,0.,0.));
#15880=DIRECTION('center_axis',(0.,1.,0.));
#15881=DIRECTION('ref_axis',(1.,0.,0.));
#15882=DIRECTION('center_axis',(0.,1.,0.));
#15883=DIRECTION('ref_axis',(1.,0.,0.));
#15884=DIRECTION('center_axis',(0.,1.,0.));
#15885=DIRECTION('ref_axis',(1.,0.,0.));
#15886=DIRECTION('center_axis',(0.,-1.,0.));
#15887=DIRECTION('ref_axis',(1.,0.,0.));
#15888=DIRECTION('center_axis',(0.,1.,0.));
#15889=DIRECTION('ref_axis',(1.,0.,0.));
#15890=DIRECTION('',(0.,-1.,0.));
#15891=DIRECTION('center_axis',(0.,1.,0.));
#15892=DIRECTION('ref_axis',(1.,0.,0.));
#15893=DIRECTION('',(0.,-1.,0.));
#15894=DIRECTION('center_axis',(0.,1.,0.));
#15895=DIRECTION('ref_axis',(1.,0.,0.));
#15896=DIRECTION('center_axis',(0.,1.,0.));
#15897=DIRECTION('ref_axis',(1.,0.,0.));
#15898=DIRECTION('center_axis',(0.,1.,0.));
#15899=DIRECTION('ref_axis',(1.,0.,0.));
#15900=DIRECTION('',(0.,-1.,0.));
#15901=DIRECTION('center_axis',(0.,1.,0.));
#15902=DIRECTION('ref_axis',(1.,0.,0.));
#15903=DIRECTION('center_axis',(0.,1.,0.));
#15904=DIRECTION('ref_axis',(1.,0.,0.));
#15905=DIRECTION('axis',(0.,0.,1.));
#15906=DIRECTION('refdir',(1.,0.,0.));
#15907=DIRECTION('center_axis',(0.,1.,0.));
#15908=DIRECTION('ref_axis',(1.,0.,0.));
#15909=DIRECTION('center_axis',(0.,-1.,0.));
#15910=DIRECTION('ref_axis',(1.,0.,0.));
#15911=DIRECTION('',(0.,-1.,0.));
#15912=DIRECTION('center_axis',(0.,-1.,0.));
#15913=DIRECTION('ref_axis',(1.,0.,0.));
#15914=DIRECTION('center_axis',(0.,1.,0.));
#15915=DIRECTION('ref_axis',(1.,0.,0.));
#15916=DIRECTION('center_axis',(0.,1.,0.));
#15917=DIRECTION('ref_axis',(1.,0.,0.));
#15918=DIRECTION('',(0.,-1.,0.));
#15919=DIRECTION('center_axis',(0.,1.,0.));
#15920=DIRECTION('ref_axis',(1.,0.,0.));
#15921=DIRECTION('center_axis',(0.,1.,0.));
#15922=DIRECTION('ref_axis',(1.,0.,0.));
#15923=DIRECTION('center_axis',(0.,1.,0.));
#15924=DIRECTION('ref_axis',(1.,0.,0.));
#15925=DIRECTION('axis',(0.,0.,1.));
#15926=DIRECTION('refdir',(1.,0.,0.));
#15927=DIRECTION('center_axis',(0.,1.,0.));
#15928=DIRECTION('ref_axis',(1.,0.,0.));
#15929=DIRECTION('center_axis',(0.,-1.,0.));
#15930=DIRECTION('ref_axis',(1.,0.,0.));
#15931=DIRECTION('',(0.,-1.,0.));
#15932=DIRECTION('center_axis',(0.,-1.,0.));
#15933=DIRECTION('ref_axis',(1.,0.,0.));
#15934=DIRECTION('center_axis',(0.,1.,0.));
#15935=DIRECTION('ref_axis',(1.,0.,0.));
#15936=DIRECTION('center_axis',(0.,1.,0.));
#15937=DIRECTION('ref_axis',(1.,0.,0.));
#15938=DIRECTION('',(0.,-1.,0.));
#15939=DIRECTION('center_axis',(0.,1.,0.));
#15940=DIRECTION('ref_axis',(1.,0.,0.));
#15941=DIRECTION('center_axis',(0.,1.,0.));
#15942=DIRECTION('ref_axis',(1.,0.,0.));
#15943=DIRECTION('center_axis',(0.,1.,0.));
#15944=DIRECTION('ref_axis',(1.,0.,0.));
#15945=DIRECTION('axis',(0.,0.,1.));
#15946=DIRECTION('refdir',(1.,0.,0.));
#15947=DIRECTION('center_axis',(0.,1.,0.));
#15948=DIRECTION('ref_axis',(1.,0.,0.));
#15949=DIRECTION('center_axis',(0.,-1.,0.));
#15950=DIRECTION('ref_axis',(1.,0.,0.));
#15951=DIRECTION('',(0.,-1.,0.));
#15952=DIRECTION('center_axis',(0.,-1.,0.));
#15953=DIRECTION('ref_axis',(1.,0.,0.));
#15954=DIRECTION('center_axis',(0.,1.,0.));
#15955=DIRECTION('ref_axis',(1.,0.,0.));
#15956=DIRECTION('center_axis',(0.,1.,0.));
#15957=DIRECTION('ref_axis',(1.,0.,0.));
#15958=DIRECTION('',(0.,-1.,0.));
#15959=DIRECTION('center_axis',(0.,1.,0.));
#15960=DIRECTION('ref_axis',(1.,0.,0.));
#15961=DIRECTION('center_axis',(0.,1.,0.));
#15962=DIRECTION('ref_axis',(1.,0.,0.));
#15963=DIRECTION('center_axis',(0.,1.,0.));
#15964=DIRECTION('ref_axis',(1.,0.,0.));
#15965=DIRECTION('axis',(0.,0.,1.));
#15966=DIRECTION('refdir',(1.,0.,0.));
#15967=DIRECTION('center_axis',(0.,1.,0.));
#15968=DIRECTION('ref_axis',(1.,0.,0.));
#15969=DIRECTION('center_axis',(0.,1.,0.));
#15970=DIRECTION('ref_axis',(1.,0.,0.));
#15971=DIRECTION('',(0.,1.,0.));
#15972=DIRECTION('center_axis',(0.,1.,0.));
#15973=DIRECTION('ref_axis',(1.,0.,0.));
#15974=DIRECTION('center_axis',(0.,1.,0.));
#15975=DIRECTION('ref_axis',(1.,0.,0.));
#15976=DIRECTION('center_axis',(0.,1.,0.));
#15977=DIRECTION('ref_axis',(1.,0.,0.));
#15978=DIRECTION('center_axis',(0.,1.,0.));
#15979=DIRECTION('ref_axis',(1.,0.,0.));
#15980=DIRECTION('',(0.,1.,0.));
#15981=DIRECTION('center_axis',(0.,-1.,0.));
#15982=DIRECTION('ref_axis',(1.,0.,0.));
#15983=DIRECTION('center_axis',(0.,1.,0.));
#15984=DIRECTION('ref_axis',(1.,0.,0.));
#15985=DIRECTION('center_axis',(0.,1.,0.));
#15986=DIRECTION('ref_axis',(1.,0.,0.));
#15987=DIRECTION('',(0.,1.,0.));
#15988=DIRECTION('center_axis',(0.,-1.,0.));
#15989=DIRECTION('ref_axis',(1.,0.,0.));
#15990=DIRECTION('center_axis',(0.,1.,0.));
#15991=DIRECTION('ref_axis',(1.,0.,0.));
#15992=DIRECTION('center_axis',(0.,1.,0.));
#15993=DIRECTION('ref_axis',(1.,0.,0.));
#15994=DIRECTION('',(0.,1.,0.));
#15995=DIRECTION('center_axis',(0.,-1.,0.));
#15996=DIRECTION('ref_axis',(1.,0.,0.));
#15997=DIRECTION('center_axis',(0.,1.,0.));
#15998=DIRECTION('ref_axis',(1.,0.,0.));
#15999=DIRECTION('center_axis',(0.,1.,0.));
#16000=DIRECTION('ref_axis',(1.,0.,0.));
#16001=DIRECTION('center_axis',(0.,1.,0.));
#16002=DIRECTION('ref_axis',(1.,0.,0.));
#16003=DIRECTION('center_axis',(0.,1.,0.));
#16004=DIRECTION('ref_axis',(1.,0.,0.));
#16005=DIRECTION('center_axis',(0.,1.,0.));
#16006=DIRECTION('ref_axis',(1.,0.,0.));
#16007=DIRECTION('center_axis',(0.,-1.,0.));
#16008=DIRECTION('ref_axis',(1.,0.,0.));
#16009=DIRECTION('center_axis',(0.,1.,0.));
#16010=DIRECTION('ref_axis',(1.,0.,0.));
#16011=DIRECTION('',(0.,-1.,0.));
#16012=DIRECTION('center_axis',(0.,1.,0.));
#16013=DIRECTION('ref_axis',(1.,0.,0.));
#16014=DIRECTION('',(0.,-1.,0.));
#16015=DIRECTION('center_axis',(0.,1.,0.));
#16016=DIRECTION('ref_axis',(1.,0.,0.));
#16017=DIRECTION('center_axis',(0.,1.,0.));
#16018=DIRECTION('ref_axis',(1.,0.,0.));
#16019=DIRECTION('center_axis',(0.,1.,0.));
#16020=DIRECTION('ref_axis',(1.,0.,0.));
#16021=DIRECTION('',(0.,-1.,0.));
#16022=DIRECTION('center_axis',(0.,1.,0.));
#16023=DIRECTION('ref_axis',(1.,0.,0.));
#16024=DIRECTION('center_axis',(0.,1.,0.));
#16025=DIRECTION('ref_axis',(1.,0.,0.));
#16026=DIRECTION('axis',(0.,0.,1.));
#16027=DIRECTION('refdir',(1.,0.,0.));
#16028=DIRECTION('center_axis',(0.,1.,0.));
#16029=DIRECTION('ref_axis',(1.,0.,0.));
#16030=DIRECTION('center_axis',(0.,-1.,0.));
#16031=DIRECTION('ref_axis',(1.,0.,0.));
#16032=DIRECTION('',(0.,-1.,0.));
#16033=DIRECTION('center_axis',(0.,-1.,0.));
#16034=DIRECTION('ref_axis',(1.,0.,0.));
#16035=DIRECTION('center_axis',(0.,1.,0.));
#16036=DIRECTION('ref_axis',(1.,0.,0.));
#16037=DIRECTION('center_axis',(0.,1.,0.));
#16038=DIRECTION('ref_axis',(1.,0.,0.));
#16039=DIRECTION('',(0.,-1.,0.));
#16040=DIRECTION('center_axis',(0.,1.,0.));
#16041=DIRECTION('ref_axis',(1.,0.,0.));
#16042=DIRECTION('center_axis',(0.,1.,0.));
#16043=DIRECTION('ref_axis',(1.,0.,0.));
#16044=DIRECTION('center_axis',(0.,1.,0.));
#16045=DIRECTION('ref_axis',(1.,0.,0.));
#16046=DIRECTION('axis',(0.,0.,1.));
#16047=DIRECTION('refdir',(1.,0.,0.));
#16048=DIRECTION('center_axis',(0.,1.,0.));
#16049=DIRECTION('ref_axis',(1.,0.,0.));
#16050=DIRECTION('center_axis',(0.,-1.,0.));
#16051=DIRECTION('ref_axis',(1.,0.,0.));
#16052=DIRECTION('',(0.,-1.,0.));
#16053=DIRECTION('center_axis',(0.,-1.,0.));
#16054=DIRECTION('ref_axis',(1.,0.,0.));
#16055=DIRECTION('center_axis',(0.,1.,0.));
#16056=DIRECTION('ref_axis',(1.,0.,0.));
#16057=DIRECTION('center_axis',(0.,1.,0.));
#16058=DIRECTION('ref_axis',(1.,0.,0.));
#16059=DIRECTION('',(0.,-1.,0.));
#16060=DIRECTION('center_axis',(0.,1.,0.));
#16061=DIRECTION('ref_axis',(1.,0.,0.));
#16062=DIRECTION('center_axis',(0.,1.,0.));
#16063=DIRECTION('ref_axis',(1.,0.,0.));
#16064=DIRECTION('center_axis',(0.,1.,0.));
#16065=DIRECTION('ref_axis',(1.,0.,0.));
#16066=DIRECTION('axis',(0.,0.,1.));
#16067=DIRECTION('refdir',(1.,0.,0.));
#16068=DIRECTION('center_axis',(0.,1.,0.));
#16069=DIRECTION('ref_axis',(1.,0.,0.));
#16070=DIRECTION('center_axis',(0.,-1.,0.));
#16071=DIRECTION('ref_axis',(1.,0.,0.));
#16072=DIRECTION('',(0.,-1.,0.));
#16073=DIRECTION('center_axis',(0.,-1.,0.));
#16074=DIRECTION('ref_axis',(1.,0.,0.));
#16075=DIRECTION('center_axis',(0.,1.,0.));
#16076=DIRECTION('ref_axis',(1.,0.,0.));
#16077=DIRECTION('center_axis',(0.,1.,0.));
#16078=DIRECTION('ref_axis',(1.,0.,0.));
#16079=DIRECTION('',(0.,-1.,0.));
#16080=DIRECTION('center_axis',(0.,1.,0.));
#16081=DIRECTION('ref_axis',(1.,0.,0.));
#16082=DIRECTION('center_axis',(0.,1.,0.));
#16083=DIRECTION('ref_axis',(1.,0.,0.));
#16084=DIRECTION('center_axis',(0.,1.,0.));
#16085=DIRECTION('ref_axis',(1.,0.,0.));
#16086=DIRECTION('axis',(0.,0.,1.));
#16087=DIRECTION('refdir',(1.,0.,0.));
#16088=DIRECTION('center_axis',(1.,0.,0.));
#16089=DIRECTION('ref_axis',(0.,0.,-1.));
#16090=DIRECTION('center_axis',(1.,0.,0.));
#16091=DIRECTION('ref_axis',(0.,0.,-1.));
#16092=DIRECTION('',(-1.,0.,0.));
#16093=DIRECTION('center_axis',(-1.,0.,0.));
#16094=DIRECTION('ref_axis',(0.,0.,-1.));
#16095=DIRECTION('',(1.,0.,0.));
#16096=DIRECTION('center_axis',(1.,0.,0.));
#16097=DIRECTION('ref_axis',(0.,0.,-1.));
#16098=DIRECTION('center_axis',(1.,0.,0.));
#16099=DIRECTION('ref_axis',(0.,0.,-1.));
#16100=DIRECTION('',(1.,0.,0.));
#16101=DIRECTION('center_axis',(-1.,0.,0.));
#16102=DIRECTION('ref_axis',(0.,0.,-1.));
#16103=DIRECTION('center_axis',(0.,0.,1.));
#16104=DIRECTION('ref_axis',(1.,0.,0.));
#16105=DIRECTION('',(0.,-1.,0.));
#16106=DIRECTION('',(1.,0.,0.));
#16107=DIRECTION('',(0.,1.,0.));
#16108=DIRECTION('center_axis',(0.,0.,-1.));
#16109=DIRECTION('ref_axis',(1.,0.,0.));
#16110=DIRECTION('center_axis',(1.,0.,0.));
#16111=DIRECTION('ref_axis',(0.,1.,0.));
#16112=DIRECTION('',(0.,0.,1.));
#16113=DIRECTION('',(0.,1.,0.));
#16114=DIRECTION('',(0.,0.,1.));
#16115=DIRECTION('',(0.,1.,0.));
#16116=DIRECTION('center_axis',(-1.,0.,0.));
#16117=DIRECTION('ref_axis',(0.,0.,-1.));
#16118=DIRECTION('center_axis',(-1.,0.,0.));
#16119=DIRECTION('ref_axis',(0.,0.,-1.));
#16120=DIRECTION('center_axis',(-1.,0.,0.));
#16121=DIRECTION('ref_axis',(0.,0.,-1.));
#16122=DIRECTION('center_axis',(0.,0.,1.));
#16123=DIRECTION('ref_axis',(1.,0.,0.));
#16124=DIRECTION('center_axis',(0.,0.,1.));
#16125=DIRECTION('ref_axis',(1.,0.,0.));
#16126=DIRECTION('',(0.,0.,1.));
#16127=DIRECTION('center_axis',(0.,0.,-1.));
#16128=DIRECTION('ref_axis',(1.,0.,0.));
#16129=DIRECTION('center_axis',(0.,0.,1.));
#16130=DIRECTION('ref_axis',(1.,0.,0.));
#16131=DIRECTION('center_axis',(0.,0.,1.));
#16132=DIRECTION('ref_axis',(1.,0.,0.));
#16133=DIRECTION('center_axis',(0.,0.,1.));
#16134=DIRECTION('ref_axis',(1.,0.,0.));
#16135=DIRECTION('center_axis',(0.,0.,1.));
#16136=DIRECTION('ref_axis',(1.,0.,0.));
#16137=DIRECTION('',(0.,0.,1.));
#16138=DIRECTION('center_axis',(0.,0.,1.));
#16139=DIRECTION('ref_axis',(1.,0.,0.));
#16140=DIRECTION('center_axis',(0.,0.,1.));
#16141=DIRECTION('ref_axis',(1.,0.,0.));
#16142=DIRECTION('',(0.,0.,1.));
#16143=DIRECTION('center_axis',(0.,0.,1.));
#16144=DIRECTION('ref_axis',(1.,0.,0.));
#16145=DIRECTION('center_axis',(0.,0.,1.));
#16146=DIRECTION('ref_axis',(1.,0.,0.));
#16147=DIRECTION('center_axis',(0.,0.,1.));
#16148=DIRECTION('ref_axis',(1.,0.,0.));
#16149=DIRECTION('center_axis',(0.,0.,1.));
#16150=DIRECTION('ref_axis',(1.,0.,0.));
#16151=DIRECTION('',(0.,0.,1.));
#16152=DIRECTION('center_axis',(1.,0.,0.));
#16153=DIRECTION('ref_axis',(0.,0.,-1.));
#16154=DIRECTION('center_axis',(1.,0.,0.));
#16155=DIRECTION('ref_axis',(0.,0.,-1.));
#16156=DIRECTION('',(1.,0.,0.));
#16157=DIRECTION('center_axis',(1.,0.,0.));
#16158=DIRECTION('ref_axis',(0.,0.,-1.));
#16159=DIRECTION('center_axis',(1.,0.,0.));
#16160=DIRECTION('ref_axis',(0.,0.,-1.));
#16161=DIRECTION('',(1.,0.,0.));
#16162=DIRECTION('center_axis',(1.,0.,0.));
#16163=DIRECTION('ref_axis',(0.,0.,-1.));
#16164=DIRECTION('center_axis',(1.,0.,0.));
#16165=DIRECTION('ref_axis',(0.,0.,-1.));
#16166=DIRECTION('',(1.,0.,0.));
#16167=DIRECTION('center_axis',(0.,1.,0.));
#16168=DIRECTION('ref_axis',(-1.,0.,0.));
#16169=DIRECTION('',(-1.,0.,0.));
#16170=DIRECTION('',(0.,0.,1.));
#16171=DIRECTION('',(-1.,0.,0.));
#16172=DIRECTION('center_axis',(0.,-1.,0.));
#16173=DIRECTION('ref_axis',(1.,0.,0.));
#16174=DIRECTION('',(1.,0.,0.));
#16175=DIRECTION('',(0.,0.,1.));
#16176=DIRECTION('center_axis',(-1.,0.,0.));
#16177=DIRECTION('ref_axis',(0.,-1.,0.));
#16178=DIRECTION('',(0.,-1.,0.));
#16179=DIRECTION('',(0.,-1.,0.));
#16180=DIRECTION('center_axis',(0.,0.,1.));
#16181=DIRECTION('ref_axis',(1.,0.,0.));
#16182=DIRECTION('center_axis',(0.,0.,1.));
#16183=DIRECTION('ref_axis',(1.,0.,0.));
#16184=DIRECTION('axis',(0.,0.,1.));
#16185=DIRECTION('refdir',(1.,0.,0.));
#16186=DIRECTION('center_axis',(1.,0.,0.));
#16187=DIRECTION('ref_axis',(0.,0.,-1.));
#16188=DIRECTION('center_axis',(1.,0.,0.));
#16189=DIRECTION('ref_axis',(0.,0.,-1.));
#16190=DIRECTION('',(1.,0.,0.));
#16191=DIRECTION('center_axis',(-1.,0.,0.));
#16192=DIRECTION('ref_axis',(0.,0.,-1.));
#16193=DIRECTION('center_axis',(1.,0.,0.));
#16194=DIRECTION('ref_axis',(0.,0.,-1.));
#16195=DIRECTION('center_axis',(1.,0.,0.));
#16196=DIRECTION('ref_axis',(0.,0.,-1.));
#16197=DIRECTION('',(1.,0.,0.));
#16198=DIRECTION('center_axis',(-1.,0.,0.));
#16199=DIRECTION('ref_axis',(0.,0.,-1.));
#16200=DIRECTION('center_axis',(1.,0.,0.));
#16201=DIRECTION('ref_axis',(0.,0.,-1.));
#16202=DIRECTION('',(-1.,0.,0.));
#16203=DIRECTION('center_axis',(-1.,0.,0.));
#16204=DIRECTION('ref_axis',(0.,0.,-1.));
#16205=DIRECTION('',(1.,0.,0.));
#16206=DIRECTION('center_axis',(1.,0.,0.));
#16207=DIRECTION('ref_axis',(0.,0.,-1.));
#16208=DIRECTION('center_axis',(1.,0.,0.));
#16209=DIRECTION('ref_axis',(0.,0.,-1.));
#16210=DIRECTION('',(-1.,0.,0.));
#16211=DIRECTION('center_axis',(-1.,0.,0.));
#16212=DIRECTION('ref_axis',(0.,0.,-1.));
#16213=DIRECTION('',(1.,0.,0.));
#16214=DIRECTION('center_axis',(1.,0.,0.));
#16215=DIRECTION('ref_axis',(0.,0.,-1.));
#16216=DIRECTION('center_axis',(1.,0.,0.));
#16217=DIRECTION('ref_axis',(0.,0.,-1.));
#16218=DIRECTION('center_axis',(1.,0.,0.));
#16219=DIRECTION('ref_axis',(0.,0.,-1.));
#16220=DIRECTION('center_axis',(1.,0.,0.));
#16221=DIRECTION('ref_axis',(0.,0.,-1.));
#16222=DIRECTION('center_axis',(-1.,0.,0.));
#16223=DIRECTION('ref_axis',(0.,0.,-1.));
#16224=DIRECTION('center_axis',(1.,0.,0.));
#16225=DIRECTION('ref_axis',(0.,0.,-1.));
#16226=DIRECTION('center_axis',(1.,0.,0.));
#16227=DIRECTION('ref_axis',(0.,0.,-1.));
#16228=DIRECTION('center_axis',(1.,0.,0.));
#16229=DIRECTION('ref_axis',(0.,-1.22464679914735E-16,1.));
#16230=DIRECTION('center_axis',(1.,0.,0.));
#16231=DIRECTION('ref_axis',(0.,0.,-1.));
#16232=DIRECTION('center_axis',(1.,0.,0.));
#16233=DIRECTION('ref_axis',(0.,0.,-1.));
#16234=DIRECTION('',(-1.,0.,0.));
#16235=DIRECTION('center_axis',(-1.,0.,0.));
#16236=DIRECTION('ref_axis',(0.,0.,-1.));
#16237=DIRECTION('center_axis',(1.,0.,0.));
#16238=DIRECTION('ref_axis',(0.,0.,-1.));
#16239=DIRECTION('axis',(0.,0.,1.));
#16240=DIRECTION('refdir',(1.,0.,0.));
#16241=DIRECTION('center_axis',(1.,0.,0.));
#16242=DIRECTION('ref_axis',(0.,0.,-1.));
#16243=DIRECTION('center_axis',(1.,0.,0.));
#16244=DIRECTION('ref_axis',(0.,0.,-1.));
#16245=DIRECTION('center_axis',(1.,0.,0.));
#16246=DIRECTION('ref_axis',(0.,0.,-1.));
#16247=DIRECTION('center_axis',(1.,0.,0.));
#16248=DIRECTION('ref_axis',(0.,0.,-1.));
#16249=DIRECTION('',(-1.,0.,0.));
#16250=DIRECTION('center_axis',(1.,0.,0.));
#16251=DIRECTION('ref_axis',(0.,0.,-1.));
#16252=DIRECTION('center_axis',(1.,0.,0.));
#16253=DIRECTION('ref_axis',(0.,0.,-1.));
#16254=DIRECTION('center_axis',(1.,0.,0.));
#16255=DIRECTION('ref_axis',(0.,0.,-1.));
#16256=DIRECTION('center_axis',(1.,0.,0.));
#16257=DIRECTION('ref_axis',(0.,0.,-1.));
#16258=DIRECTION('',(-1.,0.,0.));
#16259=DIRECTION('center_axis',(1.,0.,0.));
#16260=DIRECTION('ref_axis',(0.,0.,-1.));
#16261=DIRECTION('axis',(0.,0.,1.));
#16262=DIRECTION('refdir',(1.,0.,0.));
#16263=DIRECTION('center_axis',(1.,0.,0.));
#16264=DIRECTION('ref_axis',(0.,0.,-1.));
#16265=DIRECTION('center_axis',(1.,0.,0.));
#16266=DIRECTION('ref_axis',(0.,0.,-1.));
#16267=DIRECTION('center_axis',(1.,0.,0.));
#16268=DIRECTION('ref_axis',(0.,0.,-1.));
#16269=DIRECTION('center_axis',(1.,0.,0.));
#16270=DIRECTION('ref_axis',(0.,0.,-1.));
#16271=DIRECTION('',(-1.,0.,0.));
#16272=DIRECTION('center_axis',(1.,0.,0.));
#16273=DIRECTION('ref_axis',(0.,0.,-1.));
#16274=DIRECTION('center_axis',(1.,0.,0.));
#16275=DIRECTION('ref_axis',(0.,0.,-1.));
#16276=DIRECTION('center_axis',(1.,0.,0.));
#16277=DIRECTION('ref_axis',(0.,0.,-1.));
#16278=DIRECTION('center_axis',(1.,0.,0.));
#16279=DIRECTION('ref_axis',(0.,0.,-1.));
#16280=DIRECTION('',(-1.,0.,0.));
#16281=DIRECTION('center_axis',(1.,0.,0.));
#16282=DIRECTION('ref_axis',(0.,0.,-1.));
#16283=DIRECTION('axis',(0.,0.,1.));
#16284=DIRECTION('refdir',(1.,0.,0.));
#16285=DIRECTION('center_axis',(1.,0.,0.));
#16286=DIRECTION('ref_axis',(0.,0.,-1.));
#16287=DIRECTION('center_axis',(1.,0.,0.));
#16288=DIRECTION('ref_axis',(0.,0.,-1.));
#16289=DIRECTION('',(1.,0.,0.));
#16290=DIRECTION('center_axis',(-1.,0.,0.));
#16291=DIRECTION('ref_axis',(0.,0.,-1.));
#16292=DIRECTION('center_axis',(1.,0.,0.));
#16293=DIRECTION('ref_axis',(0.,0.,-1.));
#16294=DIRECTION('center_axis',(1.,0.,0.));
#16295=DIRECTION('ref_axis',(0.,0.,-1.));
#16296=DIRECTION('',(1.,0.,0.));
#16297=DIRECTION('center_axis',(-1.,0.,0.));
#16298=DIRECTION('ref_axis',(0.,0.,-1.));
#16299=DIRECTION('center_axis',(1.,0.,0.));
#16300=DIRECTION('ref_axis',(0.,0.,-1.));
#16301=DIRECTION('',(-1.,0.,0.));
#16302=DIRECTION('center_axis',(-1.,0.,0.));
#16303=DIRECTION('ref_axis',(0.,0.,-1.));
#16304=DIRECTION('',(1.,0.,0.));
#16305=DIRECTION('center_axis',(1.,0.,0.));
#16306=DIRECTION('ref_axis',(0.,0.,-1.));
#16307=DIRECTION('center_axis',(1.,0.,0.));
#16308=DIRECTION('ref_axis',(0.,0.,-1.));
#16309=DIRECTION('',(-1.,0.,0.));
#16310=DIRECTION('center_axis',(-1.,0.,0.));
#16311=DIRECTION('ref_axis',(0.,0.,-1.));
#16312=DIRECTION('',(1.,0.,0.));
#16313=DIRECTION('center_axis',(1.,0.,0.));
#16314=DIRECTION('ref_axis',(0.,0.,-1.));
#16315=DIRECTION('center_axis',(1.,0.,0.));
#16316=DIRECTION('ref_axis',(0.,0.,-1.));
#16317=DIRECTION('center_axis',(1.,0.,0.));
#16318=DIRECTION('ref_axis',(0.,0.,-1.));
#16319=DIRECTION('center_axis',(1.,0.,0.));
#16320=DIRECTION('ref_axis',(0.,0.,-1.));
#16321=DIRECTION('center_axis',(-1.,0.,0.));
#16322=DIRECTION('ref_axis',(0.,0.,-1.));
#16323=DIRECTION('center_axis',(1.,0.,0.));
#16324=DIRECTION('ref_axis',(0.,0.,-1.));
#16325=DIRECTION('center_axis',(1.,0.,0.));
#16326=DIRECTION('ref_axis',(0.,0.,-1.));
#16327=DIRECTION('center_axis',(1.,0.,0.));
#16328=DIRECTION('ref_axis',(0.,-1.22464679914735E-16,1.));
#16329=DIRECTION('center_axis',(1.,0.,0.));
#16330=DIRECTION('ref_axis',(0.,0.,-1.));
#16331=DIRECTION('center_axis',(1.,0.,0.));
#16332=DIRECTION('ref_axis',(0.,0.,-1.));
#16333=DIRECTION('',(-1.,0.,0.));
#16334=DIRECTION('center_axis',(-1.,0.,0.));
#16335=DIRECTION('ref_axis',(0.,0.,-1.));
#16336=DIRECTION('center_axis',(1.,0.,0.));
#16337=DIRECTION('ref_axis',(0.,0.,-1.));
#16338=DIRECTION('axis',(0.,0.,1.));
#16339=DIRECTION('refdir',(1.,0.,0.));
#16340=DIRECTION('center_axis',(1.,0.,0.));
#16341=DIRECTION('ref_axis',(0.,0.,-1.));
#16342=DIRECTION('center_axis',(1.,0.,0.));
#16343=DIRECTION('ref_axis',(0.,0.,-1.));
#16344=DIRECTION('center_axis',(1.,0.,0.));
#16345=DIRECTION('ref_axis',(0.,0.,-1.));
#16346=DIRECTION('center_axis',(1.,0.,0.));
#16347=DIRECTION('ref_axis',(0.,0.,-1.));
#16348=DIRECTION('center_axis',(1.,0.,0.));
#16349=DIRECTION('ref_axis',(0.,0.,-1.));
#16350=DIRECTION('',(-1.,0.,0.));
#16351=DIRECTION('center_axis',(1.,0.,0.));
#16352=DIRECTION('ref_axis',(0.,0.,-1.));
#16353=DIRECTION('center_axis',(1.,0.,0.));
#16354=DIRECTION('ref_axis',(0.,0.,-1.));
#16355=DIRECTION('',(-1.,0.,0.));
#16356=DIRECTION('center_axis',(1.,0.,0.));
#16357=DIRECTION('ref_axis',(0.,0.,-1.));
#16358=DIRECTION('center_axis',(1.,0.,0.));
#16359=DIRECTION('ref_axis',(0.,0.,-1.));
#16360=DIRECTION('axis',(0.,0.,1.));
#16361=DIRECTION('refdir',(1.,0.,0.));
#16362=DIRECTION('center_axis',(1.,0.,0.));
#16363=DIRECTION('ref_axis',(0.,0.,-1.));
#16364=DIRECTION('center_axis',(1.,0.,0.));
#16365=DIRECTION('ref_axis',(0.,0.,-1.));
#16366=DIRECTION('center_axis',(1.,0.,0.));
#16367=DIRECTION('ref_axis',(0.,0.,-1.));
#16368=DIRECTION('center_axis',(1.,0.,0.));
#16369=DIRECTION('ref_axis',(0.,0.,-1.));
#16370=DIRECTION('center_axis',(1.,0.,0.));
#16371=DIRECTION('ref_axis',(0.,0.,-1.));
#16372=DIRECTION('',(-1.,0.,0.));
#16373=DIRECTION('center_axis',(1.,0.,0.));
#16374=DIRECTION('ref_axis',(0.,0.,-1.));
#16375=DIRECTION('center_axis',(1.,0.,0.));
#16376=DIRECTION('ref_axis',(0.,0.,-1.));
#16377=DIRECTION('',(-1.,0.,0.));
#16378=DIRECTION('center_axis',(1.,0.,0.));
#16379=DIRECTION('ref_axis',(0.,0.,-1.));
#16380=DIRECTION('center_axis',(1.,0.,0.));
#16381=DIRECTION('ref_axis',(0.,0.,-1.));
#16382=DIRECTION('axis',(0.,0.,1.));
#16383=DIRECTION('refdir',(1.,0.,0.));
#16384=DIRECTION('center_axis',(1.,0.,0.));
#16385=DIRECTION('ref_axis',(0.,0.,-1.));
#16386=DIRECTION('center_axis',(1.,0.,0.));
#16387=DIRECTION('ref_axis',(0.,0.,-1.));
#16388=DIRECTION('',(-1.,0.,0.));
#16389=DIRECTION('center_axis',(-1.,0.,0.));
#16390=DIRECTION('ref_axis',(0.,0.,-1.));
#16391=DIRECTION('',(1.,0.,0.));
#16392=DIRECTION('center_axis',(1.,0.,0.));
#16393=DIRECTION('ref_axis',(0.,0.,-1.));
#16394=DIRECTION('center_axis',(1.,0.,0.));
#16395=DIRECTION('ref_axis',(0.,0.,-1.));
#16396=DIRECTION('',(1.,0.,0.));
#16397=DIRECTION('center_axis',(-1.,0.,0.));
#16398=DIRECTION('ref_axis',(0.,0.,-1.));
#16399=DIRECTION('center_axis',(0.,0.,1.));
#16400=DIRECTION('ref_axis',(1.,0.,0.));
#16401=DIRECTION('',(0.,-1.,0.));
#16402=DIRECTION('',(1.,0.,0.));
#16403=DIRECTION('',(0.,1.,0.));
#16404=DIRECTION('center_axis',(0.,0.,-1.));
#16405=DIRECTION('ref_axis',(1.,0.,0.));
#16406=DIRECTION('center_axis',(1.,0.,0.));
#16407=DIRECTION('ref_axis',(0.,1.,0.));
#16408=DIRECTION('',(0.,0.,1.));
#16409=DIRECTION('',(0.,1.,0.));
#16410=DIRECTION('',(0.,0.,1.));
#16411=DIRECTION('',(0.,1.,0.));
#16412=DIRECTION('center_axis',(-1.,0.,0.));
#16413=DIRECTION('ref_axis',(0.,0.,-1.));
#16414=DIRECTION('center_axis',(-1.,0.,0.));
#16415=DIRECTION('ref_axis',(0.,0.,-1.));
#16416=DIRECTION('center_axis',(-1.,0.,0.));
#16417=DIRECTION('ref_axis',(0.,0.,-1.));
#16418=DIRECTION('center_axis',(0.,0.,1.));
#16419=DIRECTION('ref_axis',(1.,0.,0.));
#16420=DIRECTION('center_axis',(0.,0.,1.));
#16421=DIRECTION('ref_axis',(1.,0.,0.));
#16422=DIRECTION('',(0.,0.,1.));
#16423=DIRECTION('center_axis',(0.,0.,-1.));
#16424=DIRECTION('ref_axis',(1.,0.,0.));
#16425=DIRECTION('center_axis',(0.,0.,1.));
#16426=DIRECTION('ref_axis',(1.,0.,0.));
#16427=DIRECTION('center_axis',(0.,0.,1.));
#16428=DIRECTION('ref_axis',(1.,0.,0.));
#16429=DIRECTION('center_axis',(0.,0.,1.));
#16430=DIRECTION('ref_axis',(1.,0.,0.));
#16431=DIRECTION('center_axis',(0.,0.,1.));
#16432=DIRECTION('ref_axis',(1.,0.,0.));
#16433=DIRECTION('',(0.,0.,1.));
#16434=DIRECTION('center_axis',(0.,0.,1.));
#16435=DIRECTION('ref_axis',(1.,0.,0.));
#16436=DIRECTION('center_axis',(0.,0.,1.));
#16437=DIRECTION('ref_axis',(1.,0.,0.));
#16438=DIRECTION('',(0.,0.,1.));
#16439=DIRECTION('center_axis',(0.,0.,1.));
#16440=DIRECTION('ref_axis',(1.,0.,0.));
#16441=DIRECTION('center_axis',(0.,0.,1.));
#16442=DIRECTION('ref_axis',(1.,0.,0.));
#16443=DIRECTION('center_axis',(0.,0.,1.));
#16444=DIRECTION('ref_axis',(1.,0.,0.));
#16445=DIRECTION('center_axis',(0.,0.,1.));
#16446=DIRECTION('ref_axis',(1.,0.,0.));
#16447=DIRECTION('',(0.,0.,1.));
#16448=DIRECTION('center_axis',(1.,0.,0.));
#16449=DIRECTION('ref_axis',(0.,0.,-1.));
#16450=DIRECTION('center_axis',(1.,0.,0.));
#16451=DIRECTION('ref_axis',(0.,0.,-1.));
#16452=DIRECTION('',(1.,0.,0.));
#16453=DIRECTION('center_axis',(1.,0.,0.));
#16454=DIRECTION('ref_axis',(0.,0.,-1.));
#16455=DIRECTION('center_axis',(1.,0.,0.));
#16456=DIRECTION('ref_axis',(0.,0.,-1.));
#16457=DIRECTION('',(1.,0.,0.));
#16458=DIRECTION('center_axis',(1.,0.,0.));
#16459=DIRECTION('ref_axis',(0.,0.,-1.));
#16460=DIRECTION('center_axis',(1.,0.,0.));
#16461=DIRECTION('ref_axis',(0.,0.,-1.));
#16462=DIRECTION('',(1.,0.,0.));
#16463=DIRECTION('center_axis',(0.,1.,0.));
#16464=DIRECTION('ref_axis',(-1.,0.,0.));
#16465=DIRECTION('',(-1.,0.,0.));
#16466=DIRECTION('',(0.,0.,1.));
#16467=DIRECTION('',(-1.,0.,0.));
#16468=DIRECTION('center_axis',(0.,-1.,0.));
#16469=DIRECTION('ref_axis',(1.,0.,0.));
#16470=DIRECTION('',(1.,0.,0.));
#16471=DIRECTION('',(0.,0.,1.));
#16472=DIRECTION('center_axis',(-1.,0.,0.));
#16473=DIRECTION('ref_axis',(0.,-1.,0.));
#16474=DIRECTION('',(0.,-1.,0.));
#16475=DIRECTION('',(0.,-1.,0.));
#16476=DIRECTION('center_axis',(0.,0.,1.));
#16477=DIRECTION('ref_axis',(1.,0.,0.));
#16478=DIRECTION('center_axis',(0.,0.,1.));
#16479=DIRECTION('ref_axis',(1.,0.,0.));
#16480=DIRECTION('axis',(0.,0.,1.));
#16481=DIRECTION('refdir',(1.,0.,0.));
#16482=DIRECTION('center_axis',(1.,0.,0.));
#16483=DIRECTION('ref_axis',(0.,0.,-1.));
#16484=DIRECTION('center_axis',(1.,0.,0.));
#16485=DIRECTION('ref_axis',(0.,0.,-1.));
#16486=DIRECTION('',(1.,0.,0.));
#16487=DIRECTION('center_axis',(-1.,0.,0.));
#16488=DIRECTION('ref_axis',(0.,0.,-1.));
#16489=DIRECTION('center_axis',(1.,0.,0.));
#16490=DIRECTION('ref_axis',(0.,0.,-1.));
#16491=DIRECTION('center_axis',(1.,0.,0.));
#16492=DIRECTION('ref_axis',(0.,0.,-1.));
#16493=DIRECTION('',(1.,0.,0.));
#16494=DIRECTION('center_axis',(-1.,0.,0.));
#16495=DIRECTION('ref_axis',(0.,0.,-1.));
#16496=DIRECTION('center_axis',(1.,0.,0.));
#16497=DIRECTION('ref_axis',(0.,0.,-1.));
#16498=DIRECTION('',(-1.,0.,0.));
#16499=DIRECTION('center_axis',(-1.,0.,0.));
#16500=DIRECTION('ref_axis',(0.,0.,-1.));
#16501=DIRECTION('',(1.,0.,0.));
#16502=DIRECTION('center_axis',(1.,0.,0.));
#16503=DIRECTION('ref_axis',(0.,0.,-1.));
#16504=DIRECTION('center_axis',(1.,0.,0.));
#16505=DIRECTION('ref_axis',(0.,0.,-1.));
#16506=DIRECTION('',(-1.,0.,0.));
#16507=DIRECTION('center_axis',(-1.,0.,0.));
#16508=DIRECTION('ref_axis',(0.,0.,-1.));
#16509=DIRECTION('',(1.,0.,0.));
#16510=DIRECTION('center_axis',(1.,0.,0.));
#16511=DIRECTION('ref_axis',(0.,0.,-1.));
#16512=DIRECTION('center_axis',(1.,0.,0.));
#16513=DIRECTION('ref_axis',(0.,0.,-1.));
#16514=DIRECTION('center_axis',(1.,0.,0.));
#16515=DIRECTION('ref_axis',(0.,0.,-1.));
#16516=DIRECTION('center_axis',(1.,0.,0.));
#16517=DIRECTION('ref_axis',(0.,0.,-1.));
#16518=DIRECTION('center_axis',(-1.,0.,0.));
#16519=DIRECTION('ref_axis',(0.,0.,-1.));
#16520=DIRECTION('center_axis',(1.,0.,0.));
#16521=DIRECTION('ref_axis',(0.,0.,-1.));
#16522=DIRECTION('center_axis',(1.,0.,0.));
#16523=DIRECTION('ref_axis',(0.,0.,-1.));
#16524=DIRECTION('center_axis',(1.,0.,0.));
#16525=DIRECTION('ref_axis',(0.,-1.22464679914735E-16,1.));
#16526=DIRECTION('center_axis',(1.,0.,0.));
#16527=DIRECTION('ref_axis',(0.,0.,-1.));
#16528=DIRECTION('center_axis',(1.,0.,0.));
#16529=DIRECTION('ref_axis',(0.,0.,-1.));
#16530=DIRECTION('',(-1.,0.,0.));
#16531=DIRECTION('center_axis',(-1.,0.,0.));
#16532=DIRECTION('ref_axis',(0.,0.,-1.));
#16533=DIRECTION('center_axis',(1.,0.,0.));
#16534=DIRECTION('ref_axis',(0.,0.,-1.));
#16535=DIRECTION('axis',(0.,0.,1.));
#16536=DIRECTION('refdir',(1.,0.,0.));
#16537=DIRECTION('center_axis',(1.,0.,0.));
#16538=DIRECTION('ref_axis',(0.,0.,-1.));
#16539=DIRECTION('center_axis',(1.,0.,0.));
#16540=DIRECTION('ref_axis',(0.,0.,-1.));
#16541=DIRECTION('center_axis',(1.,0.,0.));
#16542=DIRECTION('ref_axis',(0.,0.,-1.));
#16543=DIRECTION('center_axis',(1.,0.,0.));
#16544=DIRECTION('ref_axis',(0.,0.,-1.));
#16545=DIRECTION('',(-1.,0.,0.));
#16546=DIRECTION('center_axis',(1.,0.,0.));
#16547=DIRECTION('ref_axis',(0.,0.,-1.));
#16548=DIRECTION('center_axis',(1.,0.,0.));
#16549=DIRECTION('ref_axis',(0.,0.,-1.));
#16550=DIRECTION('center_axis',(1.,0.,0.));
#16551=DIRECTION('ref_axis',(0.,0.,-1.));
#16552=DIRECTION('center_axis',(1.,0.,0.));
#16553=DIRECTION('ref_axis',(0.,0.,-1.));
#16554=DIRECTION('',(-1.,0.,0.));
#16555=DIRECTION('center_axis',(1.,0.,0.));
#16556=DIRECTION('ref_axis',(0.,0.,-1.));
#16557=DIRECTION('axis',(0.,0.,1.));
#16558=DIRECTION('refdir',(1.,0.,0.));
#16559=DIRECTION('center_axis',(1.,0.,0.));
#16560=DIRECTION('ref_axis',(0.,0.,-1.));
#16561=DIRECTION('center_axis',(1.,0.,0.));
#16562=DIRECTION('ref_axis',(0.,0.,-1.));
#16563=DIRECTION('center_axis',(1.,0.,0.));
#16564=DIRECTION('ref_axis',(0.,0.,-1.));
#16565=DIRECTION('center_axis',(1.,0.,0.));
#16566=DIRECTION('ref_axis',(0.,0.,-1.));
#16567=DIRECTION('',(-1.,0.,0.));
#16568=DIRECTION('center_axis',(1.,0.,0.));
#16569=DIRECTION('ref_axis',(0.,0.,-1.));
#16570=DIRECTION('center_axis',(1.,0.,0.));
#16571=DIRECTION('ref_axis',(0.,0.,-1.));
#16572=DIRECTION('center_axis',(1.,0.,0.));
#16573=DIRECTION('ref_axis',(0.,0.,-1.));
#16574=DIRECTION('center_axis',(1.,0.,0.));
#16575=DIRECTION('ref_axis',(0.,0.,-1.));
#16576=DIRECTION('',(-1.,0.,0.));
#16577=DIRECTION('center_axis',(1.,0.,0.));
#16578=DIRECTION('ref_axis',(0.,0.,-1.));
#16579=DIRECTION('axis',(0.,0.,1.));
#16580=DIRECTION('refdir',(1.,0.,0.));
#16581=DIRECTION('center_axis',(1.,0.,0.));
#16582=DIRECTION('ref_axis',(0.,0.,-1.));
#16583=DIRECTION('center_axis',(1.,0.,0.));
#16584=DIRECTION('ref_axis',(0.,0.,-1.));
#16585=DIRECTION('',(1.,0.,0.));
#16586=DIRECTION('center_axis',(-1.,0.,0.));
#16587=DIRECTION('ref_axis',(0.,0.,-1.));
#16588=DIRECTION('center_axis',(1.,0.,0.));
#16589=DIRECTION('ref_axis',(0.,0.,-1.));
#16590=DIRECTION('center_axis',(1.,0.,0.));
#16591=DIRECTION('ref_axis',(0.,0.,-1.));
#16592=DIRECTION('',(1.,0.,0.));
#16593=DIRECTION('center_axis',(-1.,0.,0.));
#16594=DIRECTION('ref_axis',(0.,0.,-1.));
#16595=DIRECTION('center_axis',(1.,0.,0.));
#16596=DIRECTION('ref_axis',(0.,0.,-1.));
#16597=DIRECTION('',(-1.,0.,0.));
#16598=DIRECTION('center_axis',(-1.,0.,0.));
#16599=DIRECTION('ref_axis',(0.,0.,-1.));
#16600=DIRECTION('',(1.,0.,0.));
#16601=DIRECTION('center_axis',(1.,0.,0.));
#16602=DIRECTION('ref_axis',(0.,0.,-1.));
#16603=DIRECTION('center_axis',(1.,0.,0.));
#16604=DIRECTION('ref_axis',(0.,0.,-1.));
#16605=DIRECTION('',(-1.,0.,0.));
#16606=DIRECTION('center_axis',(-1.,0.,0.));
#16607=DIRECTION('ref_axis',(0.,0.,-1.));
#16608=DIRECTION('',(1.,0.,0.));
#16609=DIRECTION('center_axis',(1.,0.,0.));
#16610=DIRECTION('ref_axis',(0.,0.,-1.));
#16611=DIRECTION('center_axis',(1.,0.,0.));
#16612=DIRECTION('ref_axis',(0.,0.,-1.));
#16613=DIRECTION('center_axis',(1.,0.,0.));
#16614=DIRECTION('ref_axis',(0.,0.,-1.));
#16615=DIRECTION('center_axis',(1.,0.,0.));
#16616=DIRECTION('ref_axis',(0.,0.,-1.));
#16617=DIRECTION('center_axis',(-1.,0.,0.));
#16618=DIRECTION('ref_axis',(0.,0.,-1.));
#16619=DIRECTION('center_axis',(1.,0.,0.));
#16620=DIRECTION('ref_axis',(0.,0.,-1.));
#16621=DIRECTION('center_axis',(1.,0.,0.));
#16622=DIRECTION('ref_axis',(0.,0.,-1.));
#16623=DIRECTION('center_axis',(1.,0.,0.));
#16624=DIRECTION('ref_axis',(0.,-1.22464679914735E-16,1.));
#16625=DIRECTION('center_axis',(1.,0.,0.));
#16626=DIRECTION('ref_axis',(0.,0.,-1.));
#16627=DIRECTION('center_axis',(1.,0.,0.));
#16628=DIRECTION('ref_axis',(0.,0.,-1.));
#16629=DIRECTION('',(-1.,0.,0.));
#16630=DIRECTION('center_axis',(-1.,0.,0.));
#16631=DIRECTION('ref_axis',(0.,0.,-1.));
#16632=DIRECTION('center_axis',(1.,0.,0.));
#16633=DIRECTION('ref_axis',(0.,0.,-1.));
#16634=DIRECTION('axis',(0.,0.,1.));
#16635=DIRECTION('refdir',(1.,0.,0.));
#16636=DIRECTION('center_axis',(1.,0.,0.));
#16637=DIRECTION('ref_axis',(0.,0.,-1.));
#16638=DIRECTION('center_axis',(1.,0.,0.));
#16639=DIRECTION('ref_axis',(0.,0.,-1.));
#16640=DIRECTION('center_axis',(1.,0.,0.));
#16641=DIRECTION('ref_axis',(0.,0.,-1.));
#16642=DIRECTION('center_axis',(1.,0.,0.));
#16643=DIRECTION('ref_axis',(0.,0.,-1.));
#16644=DIRECTION('center_axis',(1.,0.,0.));
#16645=DIRECTION('ref_axis',(0.,0.,-1.));
#16646=DIRECTION('',(-1.,0.,0.));
#16647=DIRECTION('center_axis',(1.,0.,0.));
#16648=DIRECTION('ref_axis',(0.,0.,-1.));
#16649=DIRECTION('center_axis',(1.,0.,0.));
#16650=DIRECTION('ref_axis',(0.,0.,-1.));
#16651=DIRECTION('',(-1.,0.,0.));
#16652=DIRECTION('center_axis',(1.,0.,0.));
#16653=DIRECTION('ref_axis',(0.,0.,-1.));
#16654=DIRECTION('center_axis',(1.,0.,0.));
#16655=DIRECTION('ref_axis',(0.,0.,-1.));
#16656=DIRECTION('axis',(0.,0.,1.));
#16657=DIRECTION('refdir',(1.,0.,0.));
#16658=DIRECTION('center_axis',(1.,0.,0.));
#16659=DIRECTION('ref_axis',(0.,0.,-1.));
#16660=DIRECTION('center_axis',(1.,0.,0.));
#16661=DIRECTION('ref_axis',(0.,0.,-1.));
#16662=DIRECTION('center_axis',(1.,0.,0.));
#16663=DIRECTION('ref_axis',(0.,0.,-1.));
#16664=DIRECTION('center_axis',(1.,0.,0.));
#16665=DIRECTION('ref_axis',(0.,0.,-1.));
#16666=DIRECTION('center_axis',(1.,0.,0.));
#16667=DIRECTION('ref_axis',(0.,0.,-1.));
#16668=DIRECTION('',(-1.,0.,0.));
#16669=DIRECTION('center_axis',(1.,0.,0.));
#16670=DIRECTION('ref_axis',(0.,0.,-1.));
#16671=DIRECTION('center_axis',(1.,0.,0.));
#16672=DIRECTION('ref_axis',(0.,0.,-1.));
#16673=DIRECTION('',(-1.,0.,0.));
#16674=DIRECTION('center_axis',(1.,0.,0.));
#16675=DIRECTION('ref_axis',(0.,0.,-1.));
#16676=DIRECTION('center_axis',(1.,0.,0.));
#16677=DIRECTION('ref_axis',(0.,0.,-1.));
#16678=DIRECTION('axis',(0.,0.,1.));
#16679=DIRECTION('refdir',(1.,0.,0.));
#16680=DIRECTION('center_axis',(1.,0.,0.));
#16681=DIRECTION('ref_axis',(0.,0.,-1.));
#16682=DIRECTION('center_axis',(1.,0.,0.));
#16683=DIRECTION('ref_axis',(0.,0.,-1.));
#16684=DIRECTION('',(-1.,0.,0.));
#16685=DIRECTION('center_axis',(1.,0.,0.));
#16686=DIRECTION('ref_axis',(0.,0.,-1.));
#16687=DIRECTION('center_axis',(1.,0.,0.));
#16688=DIRECTION('ref_axis',(0.,0.,-1.));
#16689=DIRECTION('center_axis',(1.,0.,0.));
#16690=DIRECTION('ref_axis',(0.,0.,-1.));
#16691=DIRECTION('axis',(0.,0.,1.));
#16692=DIRECTION('refdir',(1.,0.,0.));
#16693=DIRECTION('center_axis',(1.,0.,0.));
#16694=DIRECTION('ref_axis',(0.,0.,-1.));
#16695=DIRECTION('center_axis',(1.,0.,0.));
#16696=DIRECTION('ref_axis',(0.,0.,-1.));
#16697=DIRECTION('',(-1.,0.,0.));
#16698=DIRECTION('center_axis',(1.,0.,0.));
#16699=DIRECTION('ref_axis',(0.,0.,-1.));
#16700=DIRECTION('center_axis',(1.,0.,0.));
#16701=DIRECTION('ref_axis',(0.,0.,-1.));
#16702=DIRECTION('center_axis',(1.,0.,0.));
#16703=DIRECTION('ref_axis',(0.,0.,-1.));
#16704=DIRECTION('axis',(0.,0.,1.));
#16705=DIRECTION('refdir',(1.,0.,0.));
#16706=DIRECTION('center_axis',(0.,1.,0.));
#16707=DIRECTION('ref_axis',(0.,0.,1.));
#16708=DIRECTION('center_axis',(0.,-1.,0.));
#16709=DIRECTION('ref_axis',(1.,0.,0.));
#16710=DIRECTION('center_axis',(0.,-1.,0.));
#16711=DIRECTION('ref_axis',(1.,0.,0.));
#16712=DIRECTION('center_axis',(0.,-1.,0.));
#16713=DIRECTION('ref_axis',(1.,0.,0.));
#16714=DIRECTION('',(0.707106781186548,0.707106781186547,8.65956056235493E-17));
#16715=DIRECTION('center_axis',(0.,-1.,0.));
#16716=DIRECTION('ref_axis',(1.,0.,0.));
#16717=DIRECTION('center_axis',(0.,-1.,0.));
#16718=DIRECTION('ref_axis',(1.,0.,0.));
#16719=DIRECTION('',(0.,1.,0.));
#16720=DIRECTION('center_axis',(0.,1.,0.));
#16721=DIRECTION('ref_axis',(1.,0.,0.));
#16722=DIRECTION('center_axis',(0.,-1.,0.));
#16723=DIRECTION('ref_axis',(1.,0.,0.));
#16724=DIRECTION('',(-0.707106781186547,0.707106781186548,-8.65956056235493E-17));
#16725=DIRECTION('center_axis',(0.,-1.,0.));
#16726=DIRECTION('ref_axis',(0.,0.,-1.));
#16727=DIRECTION('center_axis',(0.,-1.,0.));
#16728=DIRECTION('ref_axis',(1.,0.,0.));
#16729=DIRECTION('center_axis',(0.,1.,0.));
#16730=DIRECTION('ref_axis',(1.,0.,0.));
#16731=DIRECTION('center_axis',(0.,1.,0.));
#16732=DIRECTION('ref_axis',(1.,0.,0.));
#16733=DIRECTION('',(-0.447213595499958,0.894427190999916,-5.47678698264203E-17));
#16734=DIRECTION('center_axis',(0.,-1.,0.));
#16735=DIRECTION('ref_axis',(1.,0.,0.));
#16736=DIRECTION('center_axis',(0.,1.,0.));
#16737=DIRECTION('ref_axis',(1.,0.,0.));
#16738=DIRECTION('',(0.,1.,0.));
#16739=DIRECTION('center_axis',(0.,1.,0.));
#16740=DIRECTION('ref_axis',(1.,0.,0.));
#16741=DIRECTION('center_axis',(0.,-1.,0.));
#16742=DIRECTION('ref_axis',(1.,0.,0.));
#16743=DIRECTION('',(-0.707106781186547,0.707106781186548,-8.65956056235493E-17));
#16744=DIRECTION('center_axis',(0.,-1.,0.));
#16745=DIRECTION('ref_axis',(0.,0.,-1.));
#16746=DIRECTION('center_axis',(0.866025403784439,0.,-0.5));
#16747=DIRECTION('ref_axis',(0.5,0.,0.866025403784439));
#16748=DIRECTION('',(-0.5,0.,-0.866025403784439));
#16749=DIRECTION('',(0.,-1.,0.));
#16750=DIRECTION('',(0.5,0.,0.866025403784439));
#16751=DIRECTION('',(0.,-1.,0.));
#16752=DIRECTION('center_axis',(1.20185167898973E-16,0.,-1.));
#16753=DIRECTION('ref_axis',(1.,0.,1.20185167898973E-16));
#16754=DIRECTION('',(-1.,0.,-1.20185167898973E-16));
#16755=DIRECTION('',(0.,-1.,0.));
#16756=DIRECTION('',(1.,0.,1.20185167898973E-16));
#16757=DIRECTION('center_axis',(-0.866025403784439,0.,-0.5));
#16758=DIRECTION('ref_axis',(0.5,0.,-0.866025403784439));
#16759=DIRECTION('',(-0.5,0.,0.866025403784439));
#16760=DIRECTION('',(0.,-1.,0.));
#16761=DIRECTION('',(0.5,0.,-0.866025403784439));
#16762=DIRECTION('center_axis',(-0.866025403784439,0.,0.5));
#16763=DIRECTION('ref_axis',(-0.5,0.,-0.866025403784439));
#16764=DIRECTION('',(0.5,0.,0.866025403784439));
#16765=DIRECTION('',(0.,-1.,0.));
#16766=DIRECTION('',(-0.5,0.,-0.866025403784439));
#16767=DIRECTION('center_axis',(-2.40370335797945E-16,0.,1.));
#16768=DIRECTION('ref_axis',(-1.,0.,-2.40370335797945E-16));
#16769=DIRECTION('',(1.,0.,2.40370335797945E-16));
#16770=DIRECTION('',(0.,-1.,0.));
#16771=DIRECTION('',(-1.,0.,-2.40370335797945E-16));
#16772=DIRECTION('center_axis',(0.866025403784439,0.,0.5));
#16773=DIRECTION('ref_axis',(-0.5,0.,0.866025403784439));
#16774=DIRECTION('',(0.5,0.,-0.866025403784439));
#16775=DIRECTION('',(-0.5,0.,0.866025403784439));
#16776=DIRECTION('center_axis',(0.,1.,0.));
#16777=DIRECTION('ref_axis',(1.,0.,0.));
#16778=DIRECTION('center_axis',(0.,-1.,0.));
#16779=DIRECTION('ref_axis',(0.,0.,-1.));
#16780=DIRECTION('axis',(0.,0.,1.));
#16781=DIRECTION('refdir',(1.,0.,0.));
#16782=DIRECTION('axis',(0.,0.,1.));
#16783=DIRECTION('refdir',(1.,0.,0.));
#16784=DIRECTION('center_axis',(0.,1.,0.));
#16785=DIRECTION('ref_axis',(1.,0.,0.));
#16786=DIRECTION('center_axis',(0.,1.,0.));
#16787=DIRECTION('ref_axis',(1.,0.,0.));
#16788=DIRECTION('',(0.,1.,0.));
#16789=DIRECTION('center_axis',(0.,-1.,0.));
#16790=DIRECTION('ref_axis',(1.,0.,0.));
#16791=DIRECTION('center_axis',(0.,1.,0.));
#16792=DIRECTION('ref_axis',(1.,0.,0.));
#16793=DIRECTION('center_axis',(0.,1.,0.));
#16794=DIRECTION('ref_axis',(1.,0.,0.));
#16795=DIRECTION('',(0.,1.,0.));
#16796=DIRECTION('center_axis',(0.,-1.,0.));
#16797=DIRECTION('ref_axis',(1.,0.,0.));
#16798=DIRECTION('center_axis',(0.,1.,0.));
#16799=DIRECTION('ref_axis',(1.,0.,0.));
#16800=DIRECTION('center_axis',(0.,1.,0.));
#16801=DIRECTION('ref_axis',(1.,0.,0.));
#16802=DIRECTION('',(0.,1.,0.));
#16803=DIRECTION('center_axis',(0.,-1.,0.));
#16804=DIRECTION('ref_axis',(1.,0.,0.));
#16805=DIRECTION('center_axis',(0.,1.,0.));
#16806=DIRECTION('ref_axis',(1.,0.,0.));
#16807=DIRECTION('center_axis',(0.,1.,0.));
#16808=DIRECTION('ref_axis',(1.,0.,0.));
#16809=DIRECTION('',(0.,1.,0.));
#16810=DIRECTION('center_axis',(0.,-1.,0.));
#16811=DIRECTION('ref_axis',(1.,0.,0.));
#16812=DIRECTION('center_axis',(0.,1.,0.));
#16813=DIRECTION('ref_axis',(1.,0.,0.));
#16814=DIRECTION('center_axis',(0.,1.,0.));
#16815=DIRECTION('ref_axis',(1.,0.,0.));
#16816=DIRECTION('',(0.,1.,0.));
#16817=DIRECTION('center_axis',(0.,-1.,0.));
#16818=DIRECTION('ref_axis',(1.,0.,0.));
#16819=DIRECTION('center_axis',(0.,1.,0.));
#16820=DIRECTION('ref_axis',(1.,0.,0.));
#16821=DIRECTION('',(0.,-1.,0.));
#16822=DIRECTION('center_axis',(0.,1.,0.));
#16823=DIRECTION('ref_axis',(1.,0.,0.));
#16824=DIRECTION('',(0.,1.,0.));
#16825=DIRECTION('center_axis',(0.,1.,0.));
#16826=DIRECTION('ref_axis',(1.,0.,0.));
#16827=DIRECTION('center_axis',(0.,1.,0.));
#16828=DIRECTION('ref_axis',(1.,0.,0.));
#16829=DIRECTION('',(0.939692620785908,0.,0.342020143325669));
#16830=DIRECTION('center_axis',(0.,1.,0.));
#16831=DIRECTION('ref_axis',(1.,0.,0.));
#16832=DIRECTION('',(-0.939692620785909,0.,-0.342020143325669));
#16833=DIRECTION('center_axis',(0.,1.,0.));
#16834=DIRECTION('ref_axis',(1.,0.,0.));
#16835=DIRECTION('center_axis',(0.,1.,0.));
#16836=DIRECTION('ref_axis',(1.,0.,0.));
#16837=DIRECTION('center_axis',(0.,1.,0.));
#16838=DIRECTION('ref_axis',(1.,0.,0.));
#16839=DIRECTION('center_axis',(0.,1.,0.));
#16840=DIRECTION('ref_axis',(1.,0.,0.));
#16841=DIRECTION('center_axis',(0.,1.,0.));
#16842=DIRECTION('ref_axis',(1.,0.,0.));
#16843=DIRECTION('center_axis',(-0.342020143325669,0.,0.939692620785908));
#16844=DIRECTION('ref_axis',(0.939692620785908,0.,0.342020143325669));
#16845=DIRECTION('',(0.939692620785908,0.,0.342020143325669));
#16846=DIRECTION('',(0.,-1.,0.));
#16847=DIRECTION('center_axis',(0.,1.,0.));
#16848=DIRECTION('ref_axis',(1.,0.,0.));
#16849=DIRECTION('',(0.,1.,0.));
#16850=DIRECTION('center_axis',(0.,-1.,0.));
#16851=DIRECTION('ref_axis',(1.,0.,0.));
#16852=DIRECTION('center_axis',(0.,1.,0.));
#16853=DIRECTION('ref_axis',(1.,0.,0.));
#16854=DIRECTION('',(0.,1.,0.));
#16855=DIRECTION('center_axis',(0.,-1.,0.));
#16856=DIRECTION('ref_axis',(1.,0.,0.));
#16857=DIRECTION('center_axis',(0.,1.,0.));
#16858=DIRECTION('ref_axis',(1.,0.,0.));
#16859=DIRECTION('',(0.,1.,0.));
#16860=DIRECTION('center_axis',(0.,-1.,0.));
#16861=DIRECTION('ref_axis',(1.,0.,0.));
#16862=DIRECTION('center_axis',(0.,1.,0.));
#16863=DIRECTION('ref_axis',(1.,0.,0.));
#16864=DIRECTION('',(0.,1.,0.));
#16865=DIRECTION('center_axis',(0.,-1.,0.));
#16866=DIRECTION('ref_axis',(1.,0.,0.));
#16867=DIRECTION('center_axis',(0.,1.,0.));
#16868=DIRECTION('ref_axis',(1.,0.,0.));
#16869=DIRECTION('',(0.,1.,0.));
#16870=DIRECTION('center_axis',(0.,-1.,0.));
#16871=DIRECTION('ref_axis',(1.,0.,0.));
#16872=DIRECTION('center_axis',(0.,1.,0.));
#16873=DIRECTION('ref_axis',(-0.939692620785908,0.,-0.342020143325669));
#16874=DIRECTION('',(0.,1.,0.));
#16875=DIRECTION('center_axis',(0.,1.,0.));
#16876=DIRECTION('ref_axis',(1.,0.,0.));
#16877=DIRECTION('center_axis',(0.342020143325669,0.,-0.939692620785909));
#16878=DIRECTION('ref_axis',(-0.939692620785909,0.,-0.342020143325669));
#16879=DIRECTION('',(-0.939692620785909,0.,-0.342020143325669));
#16880=DIRECTION('center_axis',(0.,1.,0.));
#16881=DIRECTION('ref_axis',(0.,0.,1.));
#16882=DIRECTION('axis',(0.,0.,1.));
#16883=DIRECTION('refdir',(1.,0.,0.));
#16884=DIRECTION('center_axis',(0.,1.,0.));
#16885=DIRECTION('ref_axis',(1.,0.,0.));
#16886=DIRECTION('center_axis',(0.,1.,0.));
#16887=DIRECTION('ref_axis',(1.,0.,0.));
#16888=DIRECTION('',(0.,1.,0.));
#16889=DIRECTION('center_axis',(0.,-1.,0.));
#16890=DIRECTION('ref_axis',(1.,0.,0.));
#16891=DIRECTION('center_axis',(0.,1.,0.));
#16892=DIRECTION('ref_axis',(1.,0.,0.));
#16893=DIRECTION('center_axis',(0.,1.,0.));
#16894=DIRECTION('ref_axis',(1.,0.,0.));
#16895=DIRECTION('',(0.,1.,0.));
#16896=DIRECTION('center_axis',(0.,-1.,0.));
#16897=DIRECTION('ref_axis',(1.,0.,0.));
#16898=DIRECTION('center_axis',(0.,1.,0.));
#16899=DIRECTION('ref_axis',(1.,0.,0.));
#16900=DIRECTION('center_axis',(0.,1.,0.));
#16901=DIRECTION('ref_axis',(1.,0.,0.));
#16902=DIRECTION('',(0.,1.,0.));
#16903=DIRECTION('center_axis',(0.,-1.,0.));
#16904=DIRECTION('ref_axis',(1.,0.,0.));
#16905=DIRECTION('center_axis',(0.,1.,0.));
#16906=DIRECTION('ref_axis',(1.,0.,0.));
#16907=DIRECTION('center_axis',(0.,1.,0.));
#16908=DIRECTION('ref_axis',(1.,0.,0.));
#16909=DIRECTION('',(0.,1.,0.));
#16910=DIRECTION('center_axis',(0.,-1.,0.));
#16911=DIRECTION('ref_axis',(1.,0.,0.));
#16912=DIRECTION('center_axis',(0.,1.,0.));
#16913=DIRECTION('ref_axis',(1.,0.,0.));
#16914=DIRECTION('center_axis',(0.,-1.,0.));
#16915=DIRECTION('ref_axis',(1.,0.,0.));
#16916=DIRECTION('',(0.,-1.,0.));
#16917=DIRECTION('center_axis',(0.,-1.,0.));
#16918=DIRECTION('ref_axis',(1.,0.,0.));
#16919=DIRECTION('center_axis',(0.,1.,0.));
#16920=DIRECTION('ref_axis',(1.,0.,0.));
#16921=DIRECTION('center_axis',(0.,1.,0.));
#16922=DIRECTION('ref_axis',(1.,0.,0.));
#16923=DIRECTION('',(0.,-1.,0.));
#16924=DIRECTION('center_axis',(0.,1.,0.));
#16925=DIRECTION('ref_axis',(1.,0.,0.));
#16926=DIRECTION('center_axis',(0.,1.,0.));
#16927=DIRECTION('ref_axis',(1.,0.,0.));
#16928=DIRECTION('center_axis',(0.,1.,0.));
#16929=DIRECTION('ref_axis',(1.,0.,0.));
#16930=DIRECTION('axis',(0.,0.,1.));
#16931=DIRECTION('refdir',(1.,0.,0.));
#16932=DIRECTION('center_axis',(0.,1.,0.));
#16933=DIRECTION('ref_axis',(1.,0.,0.));
#16934=DIRECTION('center_axis',(0.,1.,0.));
#16935=DIRECTION('ref_axis',(1.,0.,0.));
#16936=DIRECTION('center_axis',(0.,1.,0.));
#16937=DIRECTION('ref_axis',(1.,0.,0.));
#16938=DIRECTION('center_axis',(0.,1.,0.));
#16939=DIRECTION('ref_axis',(1.,0.,0.));
#16940=DIRECTION('',(0.,-1.,0.));
#16941=DIRECTION('center_axis',(0.,1.,0.));
#16942=DIRECTION('ref_axis',(1.,0.,0.));
#16943=DIRECTION('center_axis',(0.,1.,0.));
#16944=DIRECTION('ref_axis',(1.,0.,0.));
#16945=DIRECTION('center_axis',(0.,1.,0.));
#16946=DIRECTION('ref_axis',(1.,0.,0.));
#16947=DIRECTION('center_axis',(0.,1.,0.));
#16948=DIRECTION('ref_axis',(1.,0.,0.));
#16949=DIRECTION('',(0.,-1.,0.));
#16950=DIRECTION('center_axis',(0.,1.,0.));
#16951=DIRECTION('ref_axis',(1.,0.,0.));
#16952=DIRECTION('axis',(0.,0.,1.));
#16953=DIRECTION('refdir',(1.,0.,0.));
#16954=DIRECTION('center_axis',(0.,1.,0.));
#16955=DIRECTION('ref_axis',(1.,0.,0.));
#16956=DIRECTION('center_axis',(0.,1.,0.));
#16957=DIRECTION('ref_axis',(1.,0.,0.));
#16958=DIRECTION('center_axis',(0.,1.,0.));
#16959=DIRECTION('ref_axis',(1.,0.,0.));
#16960=DIRECTION('center_axis',(0.,1.,0.));
#16961=DIRECTION('ref_axis',(1.,0.,0.));
#16962=DIRECTION('',(0.,-1.,0.));
#16963=DIRECTION('center_axis',(0.,1.,0.));
#16964=DIRECTION('ref_axis',(1.,0.,0.));
#16965=DIRECTION('center_axis',(0.,1.,0.));
#16966=DIRECTION('ref_axis',(1.,0.,0.));
#16967=DIRECTION('center_axis',(0.,1.,0.));
#16968=DIRECTION('ref_axis',(1.,0.,0.));
#16969=DIRECTION('center_axis',(0.,1.,0.));
#16970=DIRECTION('ref_axis',(1.,0.,0.));
#16971=DIRECTION('',(0.,-1.,0.));
#16972=DIRECTION('center_axis',(0.,1.,0.));
#16973=DIRECTION('ref_axis',(1.,0.,0.));
#16974=DIRECTION('axis',(0.,0.,1.));
#16975=DIRECTION('refdir',(1.,0.,0.));
#16976=DIRECTION('center_axis',(0.,1.,0.));
#16977=DIRECTION('ref_axis',(1.,0.,0.));
#16978=DIRECTION('center_axis',(0.,1.,0.));
#16979=DIRECTION('ref_axis',(1.,0.,0.));
#16980=DIRECTION('center_axis',(0.,1.,0.));
#16981=DIRECTION('ref_axis',(1.,0.,0.));
#16982=DIRECTION('center_axis',(0.,1.,0.));
#16983=DIRECTION('ref_axis',(1.,0.,0.));
#16984=DIRECTION('',(0.,-1.,0.));
#16985=DIRECTION('center_axis',(0.,1.,0.));
#16986=DIRECTION('ref_axis',(1.,0.,0.));
#16987=DIRECTION('center_axis',(0.,1.,0.));
#16988=DIRECTION('ref_axis',(1.,0.,0.));
#16989=DIRECTION('center_axis',(0.,1.,0.));
#16990=DIRECTION('ref_axis',(1.,0.,0.));
#16991=DIRECTION('center_axis',(0.,1.,0.));
#16992=DIRECTION('ref_axis',(1.,0.,0.));
#16993=DIRECTION('',(0.,-1.,0.));
#16994=DIRECTION('center_axis',(0.,1.,0.));
#16995=DIRECTION('ref_axis',(1.,0.,0.));
#16996=DIRECTION('axis',(0.,0.,1.));
#16997=DIRECTION('refdir',(1.,0.,0.));
#16998=DIRECTION('center_axis',(0.,1.,0.));
#16999=DIRECTION('ref_axis',(1.,0.,0.));
#17000=DIRECTION('center_axis',(0.,1.,0.));
#17001=DIRECTION('ref_axis',(1.,0.,0.));
#17002=DIRECTION('center_axis',(0.,1.,0.));
#17003=DIRECTION('ref_axis',(1.,0.,0.));
#17004=DIRECTION('center_axis',(0.,1.,0.));
#17005=DIRECTION('ref_axis',(1.,0.,0.));
#17006=DIRECTION('',(0.,-1.,0.));
#17007=DIRECTION('center_axis',(0.,1.,0.));
#17008=DIRECTION('ref_axis',(1.,0.,0.));
#17009=DIRECTION('center_axis',(0.,1.,0.));
#17010=DIRECTION('ref_axis',(1.,0.,0.));
#17011=DIRECTION('center_axis',(0.,1.,0.));
#17012=DIRECTION('ref_axis',(1.,0.,0.));
#17013=DIRECTION('center_axis',(0.,1.,0.));
#17014=DIRECTION('ref_axis',(1.,0.,0.));
#17015=DIRECTION('',(0.,-1.,0.));
#17016=DIRECTION('center_axis',(0.,1.,0.));
#17017=DIRECTION('ref_axis',(1.,0.,0.));
#17018=DIRECTION('axis',(0.,0.,1.));
#17019=DIRECTION('refdir',(1.,0.,0.));
#17020=DIRECTION('center_axis',(0.,1.,0.));
#17021=DIRECTION('ref_axis',(1.,0.,0.));
#17022=DIRECTION('center_axis',(0.,1.,0.));
#17023=DIRECTION('ref_axis',(1.,0.,0.));
#17024=DIRECTION('',(0.,1.,0.));
#17025=DIRECTION('center_axis',(0.,-1.,0.));
#17026=DIRECTION('ref_axis',(1.,0.,0.));
#17027=DIRECTION('center_axis',(0.,1.,0.));
#17028=DIRECTION('ref_axis',(1.,0.,0.));
#17029=DIRECTION('center_axis',(0.,1.,0.));
#17030=DIRECTION('ref_axis',(1.,0.,0.));
#17031=DIRECTION('',(0.,1.,0.));
#17032=DIRECTION('center_axis',(0.,-1.,0.));
#17033=DIRECTION('ref_axis',(1.,0.,0.));
#17034=DIRECTION('center_axis',(0.,1.,0.));
#17035=DIRECTION('ref_axis',(1.,0.,0.));
#17036=DIRECTION('center_axis',(0.,1.,0.));
#17037=DIRECTION('ref_axis',(1.,0.,0.));
#17038=DIRECTION('',(0.,1.,0.));
#17039=DIRECTION('center_axis',(0.,-1.,0.));
#17040=DIRECTION('ref_axis',(1.,0.,0.));
#17041=DIRECTION('center_axis',(0.,1.,0.));
#17042=DIRECTION('ref_axis',(1.,0.,0.));
#17043=DIRECTION('center_axis',(0.,1.,0.));
#17044=DIRECTION('ref_axis',(1.,0.,0.));
#17045=DIRECTION('',(0.,1.,0.));
#17046=DIRECTION('center_axis',(0.,-1.,0.));
#17047=DIRECTION('ref_axis',(1.,0.,0.));
#17048=DIRECTION('center_axis',(0.,1.,0.));
#17049=DIRECTION('ref_axis',(1.,0.,0.));
#17050=DIRECTION('center_axis',(0.,-1.,0.));
#17051=DIRECTION('ref_axis',(1.,0.,0.));
#17052=DIRECTION('',(0.,-1.,0.));
#17053=DIRECTION('center_axis',(0.,-1.,0.));
#17054=DIRECTION('ref_axis',(1.,0.,0.));
#17055=DIRECTION('center_axis',(0.,1.,0.));
#17056=DIRECTION('ref_axis',(1.,0.,0.));
#17057=DIRECTION('center_axis',(0.,1.,0.));
#17058=DIRECTION('ref_axis',(1.,0.,0.));
#17059=DIRECTION('',(0.,-1.,0.));
#17060=DIRECTION('center_axis',(0.,1.,0.));
#17061=DIRECTION('ref_axis',(1.,0.,0.));
#17062=DIRECTION('center_axis',(0.,1.,0.));
#17063=DIRECTION('ref_axis',(1.,0.,0.));
#17064=DIRECTION('center_axis',(0.,1.,0.));
#17065=DIRECTION('ref_axis',(1.,0.,0.));
#17066=DIRECTION('axis',(0.,0.,1.));
#17067=DIRECTION('refdir',(1.,0.,0.));
#17068=DIRECTION('center_axis',(0.,1.,0.));
#17069=DIRECTION('ref_axis',(1.,0.,0.));
#17070=DIRECTION('center_axis',(0.,1.,0.));
#17071=DIRECTION('ref_axis',(1.,0.,0.));
#17072=DIRECTION('center_axis',(0.,1.,0.));
#17073=DIRECTION('ref_axis',(1.,0.,0.));
#17074=DIRECTION('center_axis',(0.,1.,0.));
#17075=DIRECTION('ref_axis',(1.,0.,0.));
#17076=DIRECTION('center_axis',(0.,1.,0.));
#17077=DIRECTION('ref_axis',(1.,0.,0.));
#17078=DIRECTION('',(0.,-1.,0.));
#17079=DIRECTION('center_axis',(0.,1.,0.));
#17080=DIRECTION('ref_axis',(1.,0.,0.));
#17081=DIRECTION('center_axis',(0.,1.,0.));
#17082=DIRECTION('ref_axis',(1.,0.,0.));
#17083=DIRECTION('',(0.,-1.,0.));
#17084=DIRECTION('center_axis',(0.,1.,0.));
#17085=DIRECTION('ref_axis',(1.,0.,0.));
#17086=DIRECTION('center_axis',(0.,1.,0.));
#17087=DIRECTION('ref_axis',(1.,0.,0.));
#17088=DIRECTION('axis',(0.,0.,1.));
#17089=DIRECTION('refdir',(1.,0.,0.));
#17090=DIRECTION('center_axis',(0.,1.,0.));
#17091=DIRECTION('ref_axis',(1.,0.,0.));
#17092=DIRECTION('center_axis',(0.,1.,0.));
#17093=DIRECTION('ref_axis',(1.,0.,0.));
#17094=DIRECTION('center_axis',(0.,1.,0.));
#17095=DIRECTION('ref_axis',(1.,0.,0.));
#17096=DIRECTION('center_axis',(0.,1.,0.));
#17097=DIRECTION('ref_axis',(1.,0.,0.));
#17098=DIRECTION('center_axis',(0.,1.,0.));
#17099=DIRECTION('ref_axis',(1.,0.,0.));
#17100=DIRECTION('',(0.,-1.,0.));
#17101=DIRECTION('center_axis',(0.,1.,0.));
#17102=DIRECTION('ref_axis',(1.,0.,0.));
#17103=DIRECTION('center_axis',(0.,1.,0.));
#17104=DIRECTION('ref_axis',(1.,0.,0.));
#17105=DIRECTION('',(0.,-1.,0.));
#17106=DIRECTION('center_axis',(0.,1.,0.));
#17107=DIRECTION('ref_axis',(1.,0.,0.));
#17108=DIRECTION('center_axis',(0.,1.,0.));
#17109=DIRECTION('ref_axis',(1.,0.,0.));
#17110=DIRECTION('axis',(0.,0.,1.));
#17111=DIRECTION('refdir',(1.,0.,0.));
#17112=DIRECTION('center_axis',(0.,1.,0.));
#17113=DIRECTION('ref_axis',(1.,0.,0.));
#17114=DIRECTION('center_axis',(0.,1.,0.));
#17115=DIRECTION('ref_axis',(1.,0.,0.));
#17116=DIRECTION('center_axis',(0.,1.,0.));
#17117=DIRECTION('ref_axis',(1.,0.,0.));
#17118=DIRECTION('center_axis',(0.,1.,0.));
#17119=DIRECTION('ref_axis',(1.,0.,0.));
#17120=DIRECTION('center_axis',(0.,1.,0.));
#17121=DIRECTION('ref_axis',(1.,0.,0.));
#17122=DIRECTION('',(0.,-1.,0.));
#17123=DIRECTION('center_axis',(0.,1.,0.));
#17124=DIRECTION('ref_axis',(1.,0.,0.));
#17125=DIRECTION('center_axis',(0.,1.,0.));
#17126=DIRECTION('ref_axis',(1.,0.,0.));
#17127=DIRECTION('',(0.,-1.,0.));
#17128=DIRECTION('center_axis',(0.,1.,0.));
#17129=DIRECTION('ref_axis',(1.,0.,0.));
#17130=DIRECTION('center_axis',(0.,1.,0.));
#17131=DIRECTION('ref_axis',(1.,0.,0.));
#17132=DIRECTION('axis',(0.,0.,1.));
#17133=DIRECTION('refdir',(1.,0.,0.));
#17134=DIRECTION('center_axis',(0.,1.,0.));
#17135=DIRECTION('ref_axis',(1.,0.,0.));
#17136=DIRECTION('center_axis',(0.,1.,0.));
#17137=DIRECTION('ref_axis',(1.,0.,0.));
#17138=DIRECTION('center_axis',(0.,1.,0.));
#17139=DIRECTION('ref_axis',(1.,0.,0.));
#17140=DIRECTION('center_axis',(0.,1.,0.));
#17141=DIRECTION('ref_axis',(1.,0.,0.));
#17142=DIRECTION('center_axis',(0.,1.,0.));
#17143=DIRECTION('ref_axis',(1.,0.,0.));
#17144=DIRECTION('',(0.,-1.,0.));
#17145=DIRECTION('center_axis',(0.,1.,0.));
#17146=DIRECTION('ref_axis',(1.,0.,0.));
#17147=DIRECTION('center_axis',(0.,1.,0.));
#17148=DIRECTION('ref_axis',(1.,0.,0.));
#17149=DIRECTION('',(0.,-1.,0.));
#17150=DIRECTION('center_axis',(0.,1.,0.));
#17151=DIRECTION('ref_axis',(1.,0.,0.));
#17152=DIRECTION('center_axis',(0.,1.,0.));
#17153=DIRECTION('ref_axis',(1.,0.,0.));
#17154=DIRECTION('axis',(0.,0.,1.));
#17155=DIRECTION('refdir',(1.,0.,0.));
#17156=DIRECTION('center_axis',(0.,1.,0.));
#17157=DIRECTION('ref_axis',(1.,0.,0.));
#17158=DIRECTION('center_axis',(0.,1.,0.));
#17159=DIRECTION('ref_axis',(1.,0.,0.));
#17160=DIRECTION('',(0.,1.,0.));
#17161=DIRECTION('center_axis',(0.,-1.,0.));
#17162=DIRECTION('ref_axis',(1.,0.,0.));
#17163=DIRECTION('center_axis',(0.,1.,0.));
#17164=DIRECTION('ref_axis',(1.,0.,0.));
#17165=DIRECTION('center_axis',(0.,1.,0.));
#17166=DIRECTION('ref_axis',(1.,0.,0.));
#17167=DIRECTION('',(0.,1.,0.));
#17168=DIRECTION('center_axis',(0.,-1.,0.));
#17169=DIRECTION('ref_axis',(1.,0.,0.));
#17170=DIRECTION('center_axis',(0.,1.,0.));
#17171=DIRECTION('ref_axis',(1.,0.,0.));
#17172=DIRECTION('center_axis',(0.,1.,0.));
#17173=DIRECTION('ref_axis',(1.,0.,0.));
#17174=DIRECTION('',(0.,1.,0.));
#17175=DIRECTION('center_axis',(0.,-1.,0.));
#17176=DIRECTION('ref_axis',(1.,0.,0.));
#17177=DIRECTION('center_axis',(0.,1.,0.));
#17178=DIRECTION('ref_axis',(1.,0.,0.));
#17179=DIRECTION('center_axis',(0.,1.,0.));
#17180=DIRECTION('ref_axis',(1.,0.,0.));
#17181=DIRECTION('',(0.,1.,0.));
#17182=DIRECTION('center_axis',(0.,-1.,0.));
#17183=DIRECTION('ref_axis',(1.,0.,0.));
#17184=DIRECTION('center_axis',(0.,1.,0.));
#17185=DIRECTION('ref_axis',(1.,0.,0.));
#17186=DIRECTION('center_axis',(0.,-1.,0.));
#17187=DIRECTION('ref_axis',(1.,0.,0.));
#17188=DIRECTION('',(0.,-1.,0.));
#17189=DIRECTION('center_axis',(0.,-1.,0.));
#17190=DIRECTION('ref_axis',(1.,0.,0.));
#17191=DIRECTION('center_axis',(0.,1.,0.));
#17192=DIRECTION('ref_axis',(1.,0.,0.));
#17193=DIRECTION('center_axis',(0.,1.,0.));
#17194=DIRECTION('ref_axis',(1.,0.,0.));
#17195=DIRECTION('',(0.,-1.,0.));
#17196=DIRECTION('center_axis',(0.,1.,0.));
#17197=DIRECTION('ref_axis',(1.,0.,0.));
#17198=DIRECTION('center_axis',(0.,1.,0.));
#17199=DIRECTION('ref_axis',(1.,0.,0.));
#17200=DIRECTION('center_axis',(0.,1.,0.));
#17201=DIRECTION('ref_axis',(1.,0.,0.));
#17202=DIRECTION('axis',(0.,0.,1.));
#17203=DIRECTION('refdir',(1.,0.,0.));
#17204=DIRECTION('center_axis',(0.,1.,0.));
#17205=DIRECTION('ref_axis',(1.,0.,0.));
#17206=DIRECTION('center_axis',(0.,1.,0.));
#17207=DIRECTION('ref_axis',(1.,0.,0.));
#17208=DIRECTION('center_axis',(0.,1.,0.));
#17209=DIRECTION('ref_axis',(1.,0.,0.));
#17210=DIRECTION('center_axis',(0.,1.,0.));
#17211=DIRECTION('ref_axis',(1.,0.,0.));
#17212=DIRECTION('',(0.,-1.,0.));
#17213=DIRECTION('center_axis',(0.,1.,0.));
#17214=DIRECTION('ref_axis',(1.,0.,0.));
#17215=DIRECTION('center_axis',(0.,1.,0.));
#17216=DIRECTION('ref_axis',(1.,0.,0.));
#17217=DIRECTION('center_axis',(0.,1.,0.));
#17218=DIRECTION('ref_axis',(1.,0.,0.));
#17219=DIRECTION('center_axis',(0.,1.,0.));
#17220=DIRECTION('ref_axis',(1.,0.,0.));
#17221=DIRECTION('',(0.,-1.,0.));
#17222=DIRECTION('center_axis',(0.,1.,0.));
#17223=DIRECTION('ref_axis',(1.,0.,0.));
#17224=DIRECTION('axis',(0.,0.,1.));
#17225=DIRECTION('refdir',(1.,0.,0.));
#17226=DIRECTION('center_axis',(0.,1.,0.));
#17227=DIRECTION('ref_axis',(1.,0.,0.));
#17228=DIRECTION('center_axis',(0.,1.,0.));
#17229=DIRECTION('ref_axis',(1.,0.,0.));
#17230=DIRECTION('center_axis',(0.,1.,0.));
#17231=DIRECTION('ref_axis',(1.,0.,0.));
#17232=DIRECTION('center_axis',(0.,1.,0.));
#17233=DIRECTION('ref_axis',(1.,0.,0.));
#17234=DIRECTION('',(0.,-1.,0.));
#17235=DIRECTION('center_axis',(0.,1.,0.));
#17236=DIRECTION('ref_axis',(1.,0.,0.));
#17237=DIRECTION('center_axis',(0.,1.,0.));
#17238=DIRECTION('ref_axis',(1.,0.,0.));
#17239=DIRECTION('center_axis',(0.,1.,0.));
#17240=DIRECTION('ref_axis',(1.,0.,0.));
#17241=DIRECTION('center_axis',(0.,1.,0.));
#17242=DIRECTION('ref_axis',(1.,0.,0.));
#17243=DIRECTION('',(0.,-1.,0.));
#17244=DIRECTION('center_axis',(0.,1.,0.));
#17245=DIRECTION('ref_axis',(1.,0.,0.));
#17246=DIRECTION('axis',(0.,0.,1.));
#17247=DIRECTION('refdir',(1.,0.,0.));
#17248=DIRECTION('center_axis',(0.,1.,0.));
#17249=DIRECTION('ref_axis',(1.,0.,0.));
#17250=DIRECTION('center_axis',(0.,1.,0.));
#17251=DIRECTION('ref_axis',(1.,0.,0.));
#17252=DIRECTION('center_axis',(0.,1.,0.));
#17253=DIRECTION('ref_axis',(1.,0.,0.));
#17254=DIRECTION('center_axis',(0.,1.,0.));
#17255=DIRECTION('ref_axis',(1.,0.,0.));
#17256=DIRECTION('',(0.,-1.,0.));
#17257=DIRECTION('center_axis',(0.,1.,0.));
#17258=DIRECTION('ref_axis',(1.,0.,0.));
#17259=DIRECTION('center_axis',(0.,1.,0.));
#17260=DIRECTION('ref_axis',(1.,0.,0.));
#17261=DIRECTION('center_axis',(0.,1.,0.));
#17262=DIRECTION('ref_axis',(1.,0.,0.));
#17263=DIRECTION('center_axis',(0.,1.,0.));
#17264=DIRECTION('ref_axis',(1.,0.,0.));
#17265=DIRECTION('',(0.,-1.,0.));
#17266=DIRECTION('center_axis',(0.,1.,0.));
#17267=DIRECTION('ref_axis',(1.,0.,0.));
#17268=DIRECTION('axis',(0.,0.,1.));
#17269=DIRECTION('refdir',(1.,0.,0.));
#17270=DIRECTION('center_axis',(0.,1.,0.));
#17271=DIRECTION('ref_axis',(1.,0.,0.));
#17272=DIRECTION('center_axis',(0.,1.,0.));
#17273=DIRECTION('ref_axis',(1.,0.,0.));
#17274=DIRECTION('center_axis',(0.,1.,0.));
#17275=DIRECTION('ref_axis',(1.,0.,0.));
#17276=DIRECTION('center_axis',(0.,1.,0.));
#17277=DIRECTION('ref_axis',(1.,0.,0.));
#17278=DIRECTION('',(0.,-1.,0.));
#17279=DIRECTION('center_axis',(0.,1.,0.));
#17280=DIRECTION('ref_axis',(1.,0.,0.));
#17281=DIRECTION('center_axis',(0.,1.,0.));
#17282=DIRECTION('ref_axis',(1.,0.,0.));
#17283=DIRECTION('center_axis',(0.,1.,0.));
#17284=DIRECTION('ref_axis',(1.,0.,0.));
#17285=DIRECTION('center_axis',(0.,1.,0.));
#17286=DIRECTION('ref_axis',(1.,0.,0.));
#17287=DIRECTION('',(0.,-1.,0.));
#17288=DIRECTION('center_axis',(0.,1.,0.));
#17289=DIRECTION('ref_axis',(1.,0.,0.));
#17290=DIRECTION('axis',(0.,0.,1.));
#17291=DIRECTION('refdir',(1.,0.,0.));
#17292=DIRECTION('center_axis',(0.,1.,0.));
#17293=DIRECTION('ref_axis',(1.,0.,0.));
#17294=DIRECTION('center_axis',(0.,1.,0.));
#17295=DIRECTION('ref_axis',(1.,0.,0.));
#17296=DIRECTION('',(0.,1.,0.));
#17297=DIRECTION('center_axis',(0.,-1.,0.));
#17298=DIRECTION('ref_axis',(1.,0.,0.));
#17299=DIRECTION('center_axis',(0.,1.,0.));
#17300=DIRECTION('ref_axis',(1.,0.,0.));
#17301=DIRECTION('center_axis',(0.,1.,0.));
#17302=DIRECTION('ref_axis',(1.,0.,0.));
#17303=DIRECTION('',(0.,1.,0.));
#17304=DIRECTION('center_axis',(0.,-1.,0.));
#17305=DIRECTION('ref_axis',(1.,0.,0.));
#17306=DIRECTION('center_axis',(0.,1.,0.));
#17307=DIRECTION('ref_axis',(1.,0.,0.));
#17308=DIRECTION('center_axis',(0.,1.,0.));
#17309=DIRECTION('ref_axis',(1.,0.,0.));
#17310=DIRECTION('',(0.,1.,0.));
#17311=DIRECTION('center_axis',(0.,-1.,0.));
#17312=DIRECTION('ref_axis',(1.,0.,0.));
#17313=DIRECTION('center_axis',(0.,1.,0.));
#17314=DIRECTION('ref_axis',(1.,0.,0.));
#17315=DIRECTION('center_axis',(0.,1.,0.));
#17316=DIRECTION('ref_axis',(1.,0.,0.));
#17317=DIRECTION('',(0.,1.,0.));
#17318=DIRECTION('center_axis',(0.,-1.,0.));
#17319=DIRECTION('ref_axis',(1.,0.,0.));
#17320=DIRECTION('center_axis',(0.,1.,0.));
#17321=DIRECTION('ref_axis',(1.,0.,0.));
#17322=DIRECTION('center_axis',(0.,-1.,0.));
#17323=DIRECTION('ref_axis',(1.,0.,0.));
#17324=DIRECTION('',(0.,-1.,0.));
#17325=DIRECTION('center_axis',(0.,-1.,0.));
#17326=DIRECTION('ref_axis',(1.,0.,0.));
#17327=DIRECTION('center_axis',(0.,1.,0.));
#17328=DIRECTION('ref_axis',(1.,0.,0.));
#17329=DIRECTION('center_axis',(0.,1.,0.));
#17330=DIRECTION('ref_axis',(1.,0.,0.));
#17331=DIRECTION('',(0.,-1.,0.));
#17332=DIRECTION('center_axis',(0.,1.,0.));
#17333=DIRECTION('ref_axis',(1.,0.,0.));
#17334=DIRECTION('center_axis',(0.,1.,0.));
#17335=DIRECTION('ref_axis',(1.,0.,0.));
#17336=DIRECTION('center_axis',(0.,1.,0.));
#17337=DIRECTION('ref_axis',(1.,0.,0.));
#17338=DIRECTION('axis',(0.,0.,1.));
#17339=DIRECTION('refdir',(1.,0.,0.));
#17340=DIRECTION('center_axis',(0.,1.,0.));
#17341=DIRECTION('ref_axis',(1.,0.,0.));
#17342=DIRECTION('center_axis',(0.,1.,0.));
#17343=DIRECTION('ref_axis',(1.,0.,0.));
#17344=DIRECTION('center_axis',(0.,1.,0.));
#17345=DIRECTION('ref_axis',(1.,0.,0.));
#17346=DIRECTION('center_axis',(0.,1.,0.));
#17347=DIRECTION('ref_axis',(1.,0.,0.));
#17348=DIRECTION('center_axis',(0.,1.,0.));
#17349=DIRECTION('ref_axis',(1.,0.,0.));
#17350=DIRECTION('',(0.,-1.,0.));
#17351=DIRECTION('center_axis',(0.,1.,0.));
#17352=DIRECTION('ref_axis',(1.,0.,0.));
#17353=DIRECTION('center_axis',(0.,1.,0.));
#17354=DIRECTION('ref_axis',(1.,0.,0.));
#17355=DIRECTION('',(0.,-1.,0.));
#17356=DIRECTION('center_axis',(0.,1.,0.));
#17357=DIRECTION('ref_axis',(1.,0.,0.));
#17358=DIRECTION('center_axis',(0.,1.,0.));
#17359=DIRECTION('ref_axis',(1.,0.,0.));
#17360=DIRECTION('axis',(0.,0.,1.));
#17361=DIRECTION('refdir',(1.,0.,0.));
#17362=DIRECTION('center_axis',(0.,1.,0.));
#17363=DIRECTION('ref_axis',(1.,0.,0.));
#17364=DIRECTION('center_axis',(0.,1.,0.));
#17365=DIRECTION('ref_axis',(1.,0.,0.));
#17366=DIRECTION('center_axis',(0.,1.,0.));
#17367=DIRECTION('ref_axis',(1.,0.,0.));
#17368=DIRECTION('center_axis',(0.,1.,0.));
#17369=DIRECTION('ref_axis',(1.,0.,0.));
#17370=DIRECTION('center_axis',(0.,1.,0.));
#17371=DIRECTION('ref_axis',(1.,0.,0.));
#17372=DIRECTION('',(0.,-1.,0.));
#17373=DIRECTION('center_axis',(0.,1.,0.));
#17374=DIRECTION('ref_axis',(1.,0.,0.));
#17375=DIRECTION('center_axis',(0.,1.,0.));
#17376=DIRECTION('ref_axis',(1.,0.,0.));
#17377=DIRECTION('',(0.,-1.,0.));
#17378=DIRECTION('center_axis',(0.,1.,0.));
#17379=DIRECTION('ref_axis',(1.,0.,0.));
#17380=DIRECTION('center_axis',(0.,1.,0.));
#17381=DIRECTION('ref_axis',(1.,0.,0.));
#17382=DIRECTION('axis',(0.,0.,1.));
#17383=DIRECTION('refdir',(1.,0.,0.));
#17384=DIRECTION('center_axis',(0.,1.,0.));
#17385=DIRECTION('ref_axis',(1.,0.,0.));
#17386=DIRECTION('center_axis',(0.,1.,0.));
#17387=DIRECTION('ref_axis',(1.,0.,0.));
#17388=DIRECTION('center_axis',(0.,1.,0.));
#17389=DIRECTION('ref_axis',(1.,0.,0.));
#17390=DIRECTION('center_axis',(0.,1.,0.));
#17391=DIRECTION('ref_axis',(1.,0.,0.));
#17392=DIRECTION('center_axis',(0.,1.,0.));
#17393=DIRECTION('ref_axis',(1.,0.,0.));
#17394=DIRECTION('',(0.,-1.,0.));
#17395=DIRECTION('center_axis',(0.,1.,0.));
#17396=DIRECTION('ref_axis',(1.,0.,0.));
#17397=DIRECTION('center_axis',(0.,1.,0.));
#17398=DIRECTION('ref_axis',(1.,0.,0.));
#17399=DIRECTION('',(0.,-1.,0.));
#17400=DIRECTION('center_axis',(0.,1.,0.));
#17401=DIRECTION('ref_axis',(1.,0.,0.));
#17402=DIRECTION('center_axis',(0.,1.,0.));
#17403=DIRECTION('ref_axis',(1.,0.,0.));
#17404=DIRECTION('axis',(0.,0.,1.));
#17405=DIRECTION('refdir',(1.,0.,0.));
#17406=DIRECTION('center_axis',(0.,1.,0.));
#17407=DIRECTION('ref_axis',(1.,0.,0.));
#17408=DIRECTION('center_axis',(0.,1.,0.));
#17409=DIRECTION('ref_axis',(1.,0.,0.));
#17410=DIRECTION('center_axis',(0.,1.,0.));
#17411=DIRECTION('ref_axis',(1.,0.,0.));
#17412=DIRECTION('center_axis',(0.,1.,0.));
#17413=DIRECTION('ref_axis',(1.,0.,0.));
#17414=DIRECTION('center_axis',(0.,1.,0.));
#17415=DIRECTION('ref_axis',(1.,0.,0.));
#17416=DIRECTION('',(0.,-1.,0.));
#17417=DIRECTION('center_axis',(0.,1.,0.));
#17418=DIRECTION('ref_axis',(1.,0.,0.));
#17419=DIRECTION('center_axis',(0.,1.,0.));
#17420=DIRECTION('ref_axis',(1.,0.,0.));
#17421=DIRECTION('',(0.,-1.,0.));
#17422=DIRECTION('center_axis',(0.,1.,0.));
#17423=DIRECTION('ref_axis',(1.,0.,0.));
#17424=DIRECTION('center_axis',(0.,1.,0.));
#17425=DIRECTION('ref_axis',(1.,0.,0.));
#17426=DIRECTION('axis',(0.,0.,1.));
#17427=DIRECTION('refdir',(1.,0.,0.));
#17428=DIRECTION('axis',(0.,0.,1.));
#17429=DIRECTION('refdir',(1.,0.,0.));
#17430=DIRECTION('center_axis',(0.,1.,0.));
#17431=DIRECTION('ref_axis',(1.,0.,0.));
#17432=DIRECTION('center_axis',(0.,1.,0.));
#17433=DIRECTION('ref_axis',(1.,0.,0.));
#17434=DIRECTION('',(0.,1.,0.));
#17435=DIRECTION('center_axis',(0.,-1.,0.));
#17436=DIRECTION('ref_axis',(1.,0.,0.));
#17437=DIRECTION('center_axis',(0.,1.,0.));
#17438=DIRECTION('ref_axis',(1.,0.,0.));
#17439=DIRECTION('center_axis',(0.,1.,0.));
#17440=DIRECTION('ref_axis',(1.,0.,0.));
#17441=DIRECTION('',(0.,1.,0.));
#17442=DIRECTION('center_axis',(0.,-1.,0.));
#17443=DIRECTION('ref_axis',(1.,0.,0.));
#17444=DIRECTION('center_axis',(0.,1.,0.));
#17445=DIRECTION('ref_axis',(1.,0.,0.));
#17446=DIRECTION('center_axis',(0.,1.,0.));
#17447=DIRECTION('ref_axis',(1.,0.,0.));
#17448=DIRECTION('',(0.,1.,0.));
#17449=DIRECTION('center_axis',(0.,-1.,0.));
#17450=DIRECTION('ref_axis',(1.,0.,0.));
#17451=DIRECTION('center_axis',(0.,1.,0.));
#17452=DIRECTION('ref_axis',(1.,0.,0.));
#17453=DIRECTION('center_axis',(0.,1.,0.));
#17454=DIRECTION('ref_axis',(1.,0.,0.));
#17455=DIRECTION('',(0.,1.,0.));
#17456=DIRECTION('center_axis',(0.,-1.,0.));
#17457=DIRECTION('ref_axis',(1.,0.,0.));
#17458=DIRECTION('center_axis',(0.,1.,0.));
#17459=DIRECTION('ref_axis',(1.,0.,0.));
#17460=DIRECTION('center_axis',(0.,1.,0.));
#17461=DIRECTION('ref_axis',(1.,0.,0.));
#17462=DIRECTION('',(0.,1.,0.));
#17463=DIRECTION('center_axis',(0.,-1.,0.));
#17464=DIRECTION('ref_axis',(1.,0.,0.));
#17465=DIRECTION('center_axis',(0.,1.,0.));
#17466=DIRECTION('ref_axis',(0.413471898601476,0.,0.910516880165816));
#17467=DIRECTION('',(0.,1.,0.));
#17468=DIRECTION('center_axis',(0.,1.,0.));
#17469=DIRECTION('ref_axis',(1.,0.,0.));
#17470=DIRECTION('',(0.,-1.,0.));
#17471=DIRECTION('center_axis',(0.,1.,0.));
#17472=DIRECTION('ref_axis',(1.,0.,0.));
#17473=DIRECTION('center_axis',(-0.910516880165816,0.,0.413471898601475));
#17474=DIRECTION('ref_axis',(0.413471898601475,0.,0.910516880165816));
#17475=DIRECTION('',(0.413471898601475,0.,0.910516880165816));
#17476=DIRECTION('',(0.,-1.,0.));
#17477=DIRECTION('',(0.413471898601475,0.,0.910516880165816));
#17478=DIRECTION('center_axis',(0.,1.,0.));
#17479=DIRECTION('ref_axis',(0.,0.,1.));
#17480=DIRECTION('',(-0.413471898601475,0.,-0.910516880165816));
#17481=DIRECTION('center_axis',(0.,1.,0.));
#17482=DIRECTION('ref_axis',(1.,0.,0.));
#17483=DIRECTION('center_axis',(0.,-1.,0.));
#17484=DIRECTION('ref_axis',(1.,0.,0.));
#17485=DIRECTION('center_axis',(0.,-1.,0.));
#17486=DIRECTION('ref_axis',(1.,0.,0.));
#17487=DIRECTION('center_axis',(0.,-1.,0.));
#17488=DIRECTION('ref_axis',(1.,0.,0.));
#17489=DIRECTION('center_axis',(0.,-1.,0.));
#17490=DIRECTION('ref_axis',(1.,0.,0.));
#17491=DIRECTION('center_axis',(0.,-1.,0.));
#17492=DIRECTION('ref_axis',(1.,0.,0.));
#17493=DIRECTION('center_axis',(0.,1.,0.));
#17494=DIRECTION('ref_axis',(1.,0.,0.));
#17495=DIRECTION('center_axis',(0.,1.,0.));
#17496=DIRECTION('ref_axis',(1.,0.,0.));
#17497=DIRECTION('',(0.,1.,0.));
#17498=DIRECTION('center_axis',(0.,1.,0.));
#17499=DIRECTION('ref_axis',(1.,0.,0.));
#17500=DIRECTION('center_axis',(0.,1.,0.));
#17501=DIRECTION('ref_axis',(1.,0.,0.));
#17502=DIRECTION('',(0.,1.,0.));
#17503=DIRECTION('center_axis',(0.,1.,0.));
#17504=DIRECTION('ref_axis',(1.,0.,0.));
#17505=DIRECTION('center_axis',(0.,1.,0.));
#17506=DIRECTION('ref_axis',(1.,0.,0.));
#17507=DIRECTION('',(0.,1.,0.));
#17508=DIRECTION('center_axis',(0.,1.,0.));
#17509=DIRECTION('ref_axis',(1.,0.,0.));
#17510=DIRECTION('center_axis',(0.,1.,0.));
#17511=DIRECTION('ref_axis',(1.,0.,0.));
#17512=DIRECTION('',(0.,1.,0.));
#17513=DIRECTION('center_axis',(0.,1.,0.));
#17514=DIRECTION('ref_axis',(1.,0.,0.));
#17515=DIRECTION('center_axis',(0.,1.,0.));
#17516=DIRECTION('ref_axis',(1.,0.,0.));
#17517=DIRECTION('',(0.,1.,0.));
#17518=DIRECTION('center_axis',(0.,1.,0.));
#17519=DIRECTION('ref_axis',(-0.413471898601474,0.,-0.910516880165817));
#17520=DIRECTION('',(0.,1.,0.));
#17521=DIRECTION('center_axis',(0.,1.,0.));
#17522=DIRECTION('ref_axis',(1.,0.,0.));
#17523=DIRECTION('center_axis',(0.910516880165816,0.,-0.413471898601475));
#17524=DIRECTION('ref_axis',(-0.413471898601475,0.,-0.910516880165816));
#17525=DIRECTION('',(-0.413471898601475,0.,-0.910516880165816));
#17526=DIRECTION('center_axis',(0.,1.,0.));
#17527=DIRECTION('ref_axis',(1.,0.,0.));
#17528=DIRECTION('axis',(0.,0.,1.));
#17529=DIRECTION('refdir',(1.,0.,0.));
#17530=DIRECTION('center_axis',(0.,1.,0.));
#17531=DIRECTION('ref_axis',(1.,0.,0.));
#17532=DIRECTION('center_axis',(0.,1.,0.));
#17533=DIRECTION('ref_axis',(1.,0.,0.));
#17534=DIRECTION('',(0.,1.,0.));
#17535=DIRECTION('center_axis',(0.,-1.,0.));
#17536=DIRECTION('ref_axis',(1.,0.,0.));
#17537=DIRECTION('center_axis',(0.,1.,0.));
#17538=DIRECTION('ref_axis',(1.,0.,0.));
#17539=DIRECTION('center_axis',(0.,1.,0.));
#17540=DIRECTION('ref_axis',(1.,0.,0.));
#17541=DIRECTION('',(0.,1.,0.));
#17542=DIRECTION('center_axis',(0.,-1.,0.));
#17543=DIRECTION('ref_axis',(1.,0.,0.));
#17544=DIRECTION('center_axis',(0.,1.,0.));
#17545=DIRECTION('ref_axis',(1.,0.,0.));
#17546=DIRECTION('center_axis',(0.,1.,0.));
#17547=DIRECTION('ref_axis',(1.,0.,0.));
#17548=DIRECTION('',(0.,1.,0.));
#17549=DIRECTION('center_axis',(0.,-1.,0.));
#17550=DIRECTION('ref_axis',(1.,0.,0.));
#17551=DIRECTION('center_axis',(0.,1.,0.));
#17552=DIRECTION('ref_axis',(1.,0.,0.));
#17553=DIRECTION('center_axis',(0.,1.,0.));
#17554=DIRECTION('ref_axis',(1.,0.,0.));
#17555=DIRECTION('',(0.,1.,0.));
#17556=DIRECTION('center_axis',(0.,-1.,0.));
#17557=DIRECTION('ref_axis',(1.,0.,0.));
#17558=DIRECTION('center_axis',(0.,1.,0.));
#17559=DIRECTION('ref_axis',(1.,0.,0.));
#17560=DIRECTION('center_axis',(0.,-1.,0.));
#17561=DIRECTION('ref_axis',(1.,0.,0.));
#17562=DIRECTION('',(0.,-1.,0.));
#17563=DIRECTION('center_axis',(0.,-1.,0.));
#17564=DIRECTION('ref_axis',(1.,0.,0.));
#17565=DIRECTION('center_axis',(0.,1.,0.));
#17566=DIRECTION('ref_axis',(1.,0.,0.));
#17567=DIRECTION('center_axis',(0.,1.,0.));
#17568=DIRECTION('ref_axis',(1.,0.,0.));
#17569=DIRECTION('',(0.,-1.,0.));
#17570=DIRECTION('center_axis',(0.,1.,0.));
#17571=DIRECTION('ref_axis',(1.,0.,0.));
#17572=DIRECTION('center_axis',(0.,1.,0.));
#17573=DIRECTION('ref_axis',(1.,0.,0.));
#17574=DIRECTION('center_axis',(0.,1.,0.));
#17575=DIRECTION('ref_axis',(1.,0.,0.));
#17576=DIRECTION('axis',(0.,0.,1.));
#17577=DIRECTION('refdir',(1.,0.,0.));
#17578=DIRECTION('center_axis',(0.,1.,0.));
#17579=DIRECTION('ref_axis',(1.,0.,0.));
#17580=DIRECTION('center_axis',(0.,1.,0.));
#17581=DIRECTION('ref_axis',(1.,0.,0.));
#17582=DIRECTION('center_axis',(0.,1.,0.));
#17583=DIRECTION('ref_axis',(1.,0.,0.));
#17584=DIRECTION('center_axis',(0.,1.,0.));
#17585=DIRECTION('ref_axis',(1.,0.,0.));
#17586=DIRECTION('',(0.,-1.,0.));
#17587=DIRECTION('center_axis',(0.,1.,0.));
#17588=DIRECTION('ref_axis',(1.,0.,0.));
#17589=DIRECTION('center_axis',(0.,1.,0.));
#17590=DIRECTION('ref_axis',(1.,0.,0.));
#17591=DIRECTION('center_axis',(0.,1.,0.));
#17592=DIRECTION('ref_axis',(1.,0.,0.));
#17593=DIRECTION('center_axis',(0.,1.,0.));
#17594=DIRECTION('ref_axis',(1.,0.,0.));
#17595=DIRECTION('',(0.,-1.,0.));
#17596=DIRECTION('center_axis',(0.,1.,0.));
#17597=DIRECTION('ref_axis',(1.,0.,0.));
#17598=DIRECTION('axis',(0.,0.,1.));
#17599=DIRECTION('refdir',(1.,0.,0.));
#17600=DIRECTION('center_axis',(0.,1.,0.));
#17601=DIRECTION('ref_axis',(1.,0.,0.));
#17602=DIRECTION('center_axis',(0.,1.,0.));
#17603=DIRECTION('ref_axis',(1.,0.,0.));
#17604=DIRECTION('center_axis',(0.,1.,0.));
#17605=DIRECTION('ref_axis',(1.,0.,0.));
#17606=DIRECTION('center_axis',(0.,1.,0.));
#17607=DIRECTION('ref_axis',(1.,0.,0.));
#17608=DIRECTION('',(0.,-1.,0.));
#17609=DIRECTION('center_axis',(0.,1.,0.));
#17610=DIRECTION('ref_axis',(1.,0.,0.));
#17611=DIRECTION('center_axis',(0.,1.,0.));
#17612=DIRECTION('ref_axis',(1.,0.,0.));
#17613=DIRECTION('center_axis',(0.,1.,0.));
#17614=DIRECTION('ref_axis',(1.,0.,0.));
#17615=DIRECTION('center_axis',(0.,1.,0.));
#17616=DIRECTION('ref_axis',(1.,0.,0.));
#17617=DIRECTION('',(0.,-1.,0.));
#17618=DIRECTION('center_axis',(0.,1.,0.));
#17619=DIRECTION('ref_axis',(1.,0.,0.));
#17620=DIRECTION('axis',(0.,0.,1.));
#17621=DIRECTION('refdir',(1.,0.,0.));
#17622=DIRECTION('center_axis',(0.,1.,0.));
#17623=DIRECTION('ref_axis',(1.,0.,0.));
#17624=DIRECTION('center_axis',(0.,1.,0.));
#17625=DIRECTION('ref_axis',(1.,0.,0.));
#17626=DIRECTION('center_axis',(0.,1.,0.));
#17627=DIRECTION('ref_axis',(1.,0.,0.));
#17628=DIRECTION('center_axis',(0.,1.,0.));
#17629=DIRECTION('ref_axis',(1.,0.,0.));
#17630=DIRECTION('',(0.,-1.,0.));
#17631=DIRECTION('center_axis',(0.,1.,0.));
#17632=DIRECTION('ref_axis',(1.,0.,0.));
#17633=DIRECTION('center_axis',(0.,1.,0.));
#17634=DIRECTION('ref_axis',(1.,0.,0.));
#17635=DIRECTION('center_axis',(0.,1.,0.));
#17636=DIRECTION('ref_axis',(1.,0.,0.));
#17637=DIRECTION('center_axis',(0.,1.,0.));
#17638=DIRECTION('ref_axis',(1.,0.,0.));
#17639=DIRECTION('',(0.,-1.,0.));
#17640=DIRECTION('center_axis',(0.,1.,0.));
#17641=DIRECTION('ref_axis',(1.,0.,0.));
#17642=DIRECTION('axis',(0.,0.,1.));
#17643=DIRECTION('refdir',(1.,0.,0.));
#17644=DIRECTION('center_axis',(0.,1.,0.));
#17645=DIRECTION('ref_axis',(1.,0.,0.));
#17646=DIRECTION('center_axis',(0.,1.,0.));
#17647=DIRECTION('ref_axis',(1.,0.,0.));
#17648=DIRECTION('center_axis',(0.,1.,0.));
#17649=DIRECTION('ref_axis',(1.,0.,0.));
#17650=DIRECTION('center_axis',(0.,1.,0.));
#17651=DIRECTION('ref_axis',(1.,0.,0.));
#17652=DIRECTION('',(0.,-1.,0.));
#17653=DIRECTION('center_axis',(0.,1.,0.));
#17654=DIRECTION('ref_axis',(1.,0.,0.));
#17655=DIRECTION('center_axis',(0.,1.,0.));
#17656=DIRECTION('ref_axis',(1.,0.,0.));
#17657=DIRECTION('center_axis',(0.,1.,0.));
#17658=DIRECTION('ref_axis',(1.,0.,0.));
#17659=DIRECTION('center_axis',(0.,1.,0.));
#17660=DIRECTION('ref_axis',(1.,0.,0.));
#17661=DIRECTION('',(0.,-1.,0.));
#17662=DIRECTION('center_axis',(0.,1.,0.));
#17663=DIRECTION('ref_axis',(1.,0.,0.));
#17664=DIRECTION('axis',(0.,0.,1.));
#17665=DIRECTION('refdir',(1.,0.,0.));
#17666=DIRECTION('center_axis',(0.,1.,0.));
#17667=DIRECTION('ref_axis',(1.,0.,0.));
#17668=DIRECTION('center_axis',(0.,1.,0.));
#17669=DIRECTION('ref_axis',(1.,0.,0.));
#17670=DIRECTION('',(0.,1.,0.));
#17671=DIRECTION('center_axis',(0.,-1.,0.));
#17672=DIRECTION('ref_axis',(1.,0.,0.));
#17673=DIRECTION('center_axis',(0.,1.,0.));
#17674=DIRECTION('ref_axis',(1.,0.,0.));
#17675=DIRECTION('center_axis',(0.,1.,0.));
#17676=DIRECTION('ref_axis',(1.,0.,0.));
#17677=DIRECTION('',(0.,1.,0.));
#17678=DIRECTION('center_axis',(0.,-1.,0.));
#17679=DIRECTION('ref_axis',(1.,0.,0.));
#17680=DIRECTION('center_axis',(0.,1.,0.));
#17681=DIRECTION('ref_axis',(1.,0.,0.));
#17682=DIRECTION('center_axis',(0.,1.,0.));
#17683=DIRECTION('ref_axis',(1.,0.,0.));
#17684=DIRECTION('',(0.,1.,0.));
#17685=DIRECTION('center_axis',(0.,-1.,0.));
#17686=DIRECTION('ref_axis',(1.,0.,0.));
#17687=DIRECTION('center_axis',(0.,1.,0.));
#17688=DIRECTION('ref_axis',(1.,0.,0.));
#17689=DIRECTION('center_axis',(0.,1.,0.));
#17690=DIRECTION('ref_axis',(1.,0.,0.));
#17691=DIRECTION('',(0.,1.,0.));
#17692=DIRECTION('center_axis',(0.,-1.,0.));
#17693=DIRECTION('ref_axis',(1.,0.,0.));
#17694=DIRECTION('center_axis',(0.,1.,0.));
#17695=DIRECTION('ref_axis',(1.,0.,0.));
#17696=DIRECTION('center_axis',(0.,-1.,0.));
#17697=DIRECTION('ref_axis',(1.,0.,0.));
#17698=DIRECTION('',(0.,-1.,0.));
#17699=DIRECTION('center_axis',(0.,-1.,0.));
#17700=DIRECTION('ref_axis',(1.,0.,0.));
#17701=DIRECTION('center_axis',(0.,1.,0.));
#17702=DIRECTION('ref_axis',(1.,0.,0.));
#17703=DIRECTION('center_axis',(0.,1.,0.));
#17704=DIRECTION('ref_axis',(1.,0.,0.));
#17705=DIRECTION('',(0.,-1.,0.));
#17706=DIRECTION('center_axis',(0.,1.,0.));
#17707=DIRECTION('ref_axis',(1.,0.,0.));
#17708=DIRECTION('center_axis',(0.,1.,0.));
#17709=DIRECTION('ref_axis',(1.,0.,0.));
#17710=DIRECTION('center_axis',(0.,1.,0.));
#17711=DIRECTION('ref_axis',(1.,0.,0.));
#17712=DIRECTION('axis',(0.,0.,1.));
#17713=DIRECTION('refdir',(1.,0.,0.));
#17714=DIRECTION('center_axis',(0.,1.,0.));
#17715=DIRECTION('ref_axis',(1.,0.,0.));
#17716=DIRECTION('center_axis',(0.,1.,0.));
#17717=DIRECTION('ref_axis',(1.,0.,0.));
#17718=DIRECTION('center_axis',(0.,1.,0.));
#17719=DIRECTION('ref_axis',(1.,0.,0.));
#17720=DIRECTION('center_axis',(0.,1.,0.));
#17721=DIRECTION('ref_axis',(1.,0.,0.));
#17722=DIRECTION('center_axis',(0.,1.,0.));
#17723=DIRECTION('ref_axis',(1.,0.,0.));
#17724=DIRECTION('',(0.,-1.,0.));
#17725=DIRECTION('center_axis',(0.,1.,0.));
#17726=DIRECTION('ref_axis',(1.,0.,0.));
#17727=DIRECTION('center_axis',(0.,1.,0.));
#17728=DIRECTION('ref_axis',(1.,0.,0.));
#17729=DIRECTION('',(0.,-1.,0.));
#17730=DIRECTION('center_axis',(0.,1.,0.));
#17731=DIRECTION('ref_axis',(1.,0.,0.));
#17732=DIRECTION('center_axis',(0.,1.,0.));
#17733=DIRECTION('ref_axis',(1.,0.,0.));
#17734=DIRECTION('axis',(0.,0.,1.));
#17735=DIRECTION('refdir',(1.,0.,0.));
#17736=DIRECTION('center_axis',(0.,1.,0.));
#17737=DIRECTION('ref_axis',(1.,0.,0.));
#17738=DIRECTION('center_axis',(0.,1.,0.));
#17739=DIRECTION('ref_axis',(1.,0.,0.));
#17740=DIRECTION('center_axis',(0.,1.,0.));
#17741=DIRECTION('ref_axis',(1.,0.,0.));
#17742=DIRECTION('center_axis',(0.,1.,0.));
#17743=DIRECTION('ref_axis',(1.,0.,0.));
#17744=DIRECTION('center_axis',(0.,1.,0.));
#17745=DIRECTION('ref_axis',(1.,0.,0.));
#17746=DIRECTION('',(0.,-1.,0.));
#17747=DIRECTION('center_axis',(0.,1.,0.));
#17748=DIRECTION('ref_axis',(1.,0.,0.));
#17749=DIRECTION('center_axis',(0.,1.,0.));
#17750=DIRECTION('ref_axis',(1.,0.,0.));
#17751=DIRECTION('',(0.,-1.,0.));
#17752=DIRECTION('center_axis',(0.,1.,0.));
#17753=DIRECTION('ref_axis',(1.,0.,0.));
#17754=DIRECTION('center_axis',(0.,1.,0.));
#17755=DIRECTION('ref_axis',(1.,0.,0.));
#17756=DIRECTION('axis',(0.,0.,1.));
#17757=DIRECTION('refdir',(1.,0.,0.));
#17758=DIRECTION('center_axis',(0.,1.,0.));
#17759=DIRECTION('ref_axis',(1.,0.,0.));
#17760=DIRECTION('center_axis',(0.,1.,0.));
#17761=DIRECTION('ref_axis',(1.,0.,0.));
#17762=DIRECTION('center_axis',(0.,1.,0.));
#17763=DIRECTION('ref_axis',(1.,0.,0.));
#17764=DIRECTION('center_axis',(0.,1.,0.));
#17765=DIRECTION('ref_axis',(1.,0.,0.));
#17766=DIRECTION('center_axis',(0.,1.,0.));
#17767=DIRECTION('ref_axis',(1.,0.,0.));
#17768=DIRECTION('',(0.,-1.,0.));
#17769=DIRECTION('center_axis',(0.,1.,0.));
#17770=DIRECTION('ref_axis',(1.,0.,0.));
#17771=DIRECTION('center_axis',(0.,1.,0.));
#17772=DIRECTION('ref_axis',(1.,0.,0.));
#17773=DIRECTION('',(0.,-1.,0.));
#17774=DIRECTION('center_axis',(0.,1.,0.));
#17775=DIRECTION('ref_axis',(1.,0.,0.));
#17776=DIRECTION('center_axis',(0.,1.,0.));
#17777=DIRECTION('ref_axis',(1.,0.,0.));
#17778=DIRECTION('axis',(0.,0.,1.));
#17779=DIRECTION('refdir',(1.,0.,0.));
#17780=DIRECTION('center_axis',(0.,1.,0.));
#17781=DIRECTION('ref_axis',(1.,0.,0.));
#17782=DIRECTION('center_axis',(0.,1.,0.));
#17783=DIRECTION('ref_axis',(1.,0.,0.));
#17784=DIRECTION('center_axis',(0.,1.,0.));
#17785=DIRECTION('ref_axis',(1.,0.,0.));
#17786=DIRECTION('center_axis',(0.,1.,0.));
#17787=DIRECTION('ref_axis',(1.,0.,0.));
#17788=DIRECTION('center_axis',(0.,1.,0.));
#17789=DIRECTION('ref_axis',(1.,0.,0.));
#17790=DIRECTION('',(0.,-1.,0.));
#17791=DIRECTION('center_axis',(0.,1.,0.));
#17792=DIRECTION('ref_axis',(1.,0.,0.));
#17793=DIRECTION('center_axis',(0.,1.,0.));
#17794=DIRECTION('ref_axis',(1.,0.,0.));
#17795=DIRECTION('',(0.,-1.,0.));
#17796=DIRECTION('center_axis',(0.,1.,0.));
#17797=DIRECTION('ref_axis',(1.,0.,0.));
#17798=DIRECTION('center_axis',(0.,1.,0.));
#17799=DIRECTION('ref_axis',(1.,0.,0.));
#17800=DIRECTION('axis',(0.,0.,1.));
#17801=DIRECTION('refdir',(1.,0.,0.));
#17802=DIRECTION('center_axis',(0.,1.,0.));
#17803=DIRECTION('ref_axis',(1.,0.,0.));
#17804=DIRECTION('center_axis',(0.,1.,0.));
#17805=DIRECTION('ref_axis',(1.,0.,0.));
#17806=DIRECTION('',(0.,1.,0.));
#17807=DIRECTION('center_axis',(0.,-1.,0.));
#17808=DIRECTION('ref_axis',(1.,0.,0.));
#17809=DIRECTION('center_axis',(0.,1.,0.));
#17810=DIRECTION('ref_axis',(1.,0.,0.));
#17811=DIRECTION('center_axis',(0.,1.,0.));
#17812=DIRECTION('ref_axis',(1.,0.,0.));
#17813=DIRECTION('',(0.,1.,0.));
#17814=DIRECTION('center_axis',(0.,-1.,0.));
#17815=DIRECTION('ref_axis',(1.,0.,0.));
#17816=DIRECTION('center_axis',(0.,1.,0.));
#17817=DIRECTION('ref_axis',(1.,0.,0.));
#17818=DIRECTION('center_axis',(0.,1.,0.));
#17819=DIRECTION('ref_axis',(1.,0.,0.));
#17820=DIRECTION('',(0.,1.,0.));
#17821=DIRECTION('center_axis',(0.,-1.,0.));
#17822=DIRECTION('ref_axis',(1.,0.,0.));
#17823=DIRECTION('center_axis',(0.,1.,0.));
#17824=DIRECTION('ref_axis',(1.,0.,0.));
#17825=DIRECTION('center_axis',(0.,1.,0.));
#17826=DIRECTION('ref_axis',(1.,0.,0.));
#17827=DIRECTION('',(0.,1.,0.));
#17828=DIRECTION('center_axis',(0.,-1.,0.));
#17829=DIRECTION('ref_axis',(1.,0.,0.));
#17830=DIRECTION('center_axis',(0.,1.,0.));
#17831=DIRECTION('ref_axis',(1.,0.,0.));
#17832=DIRECTION('center_axis',(0.,-1.,0.));
#17833=DIRECTION('ref_axis',(1.,0.,0.));
#17834=DIRECTION('',(0.,-1.,0.));
#17835=DIRECTION('center_axis',(0.,-1.,0.));
#17836=DIRECTION('ref_axis',(1.,0.,0.));
#17837=DIRECTION('center_axis',(0.,1.,0.));
#17838=DIRECTION('ref_axis',(1.,0.,0.));
#17839=DIRECTION('center_axis',(0.,1.,0.));
#17840=DIRECTION('ref_axis',(1.,0.,0.));
#17841=DIRECTION('',(0.,-1.,0.));
#17842=DIRECTION('center_axis',(0.,1.,0.));
#17843=DIRECTION('ref_axis',(1.,0.,0.));
#17844=DIRECTION('center_axis',(0.,1.,0.));
#17845=DIRECTION('ref_axis',(1.,0.,0.));
#17846=DIRECTION('center_axis',(0.,1.,0.));
#17847=DIRECTION('ref_axis',(1.,0.,0.));
#17848=DIRECTION('axis',(0.,0.,1.));
#17849=DIRECTION('refdir',(1.,0.,0.));
#17850=DIRECTION('center_axis',(0.,1.,0.));
#17851=DIRECTION('ref_axis',(1.,0.,0.));
#17852=DIRECTION('center_axis',(0.,1.,0.));
#17853=DIRECTION('ref_axis',(1.,0.,0.));
#17854=DIRECTION('center_axis',(0.,1.,0.));
#17855=DIRECTION('ref_axis',(1.,0.,0.));
#17856=DIRECTION('center_axis',(0.,1.,0.));
#17857=DIRECTION('ref_axis',(1.,0.,0.));
#17858=DIRECTION('',(0.,-1.,0.));
#17859=DIRECTION('center_axis',(0.,1.,0.));
#17860=DIRECTION('ref_axis',(1.,0.,0.));
#17861=DIRECTION('center_axis',(0.,1.,0.));
#17862=DIRECTION('ref_axis',(1.,0.,0.));
#17863=DIRECTION('center_axis',(0.,1.,0.));
#17864=DIRECTION('ref_axis',(1.,0.,0.));
#17865=DIRECTION('center_axis',(0.,1.,0.));
#17866=DIRECTION('ref_axis',(1.,0.,0.));
#17867=DIRECTION('',(0.,-1.,0.));
#17868=DIRECTION('center_axis',(0.,1.,0.));
#17869=DIRECTION('ref_axis',(1.,0.,0.));
#17870=DIRECTION('axis',(0.,0.,1.));
#17871=DIRECTION('refdir',(1.,0.,0.));
#17872=DIRECTION('center_axis',(0.,1.,0.));
#17873=DIRECTION('ref_axis',(1.,0.,0.));
#17874=DIRECTION('center_axis',(0.,1.,0.));
#17875=DIRECTION('ref_axis',(1.,0.,0.));
#17876=DIRECTION('center_axis',(0.,1.,0.));
#17877=DIRECTION('ref_axis',(1.,0.,0.));
#17878=DIRECTION('center_axis',(0.,1.,0.));
#17879=DIRECTION('ref_axis',(1.,0.,0.));
#17880=DIRECTION('',(0.,-1.,0.));
#17881=DIRECTION('center_axis',(0.,1.,0.));
#17882=DIRECTION('ref_axis',(1.,0.,0.));
#17883=DIRECTION('center_axis',(0.,1.,0.));
#17884=DIRECTION('ref_axis',(1.,0.,0.));
#17885=DIRECTION('center_axis',(0.,1.,0.));
#17886=DIRECTION('ref_axis',(1.,0.,0.));
#17887=DIRECTION('center_axis',(0.,1.,0.));
#17888=DIRECTION('ref_axis',(1.,0.,0.));
#17889=DIRECTION('',(0.,-1.,0.));
#17890=DIRECTION('center_axis',(0.,1.,0.));
#17891=DIRECTION('ref_axis',(1.,0.,0.));
#17892=DIRECTION('axis',(0.,0.,1.));
#17893=DIRECTION('refdir',(1.,0.,0.));
#17894=DIRECTION('center_axis',(0.,1.,0.));
#17895=DIRECTION('ref_axis',(1.,0.,0.));
#17896=DIRECTION('center_axis',(0.,1.,0.));
#17897=DIRECTION('ref_axis',(1.,0.,0.));
#17898=DIRECTION('center_axis',(0.,1.,0.));
#17899=DIRECTION('ref_axis',(1.,0.,0.));
#17900=DIRECTION('center_axis',(0.,1.,0.));
#17901=DIRECTION('ref_axis',(1.,0.,0.));
#17902=DIRECTION('',(0.,-1.,0.));
#17903=DIRECTION('center_axis',(0.,1.,0.));
#17904=DIRECTION('ref_axis',(1.,0.,0.));
#17905=DIRECTION('center_axis',(0.,1.,0.));
#17906=DIRECTION('ref_axis',(1.,0.,0.));
#17907=DIRECTION('center_axis',(0.,1.,0.));
#17908=DIRECTION('ref_axis',(1.,0.,0.));
#17909=DIRECTION('center_axis',(0.,1.,0.));
#17910=DIRECTION('ref_axis',(1.,0.,0.));
#17911=DIRECTION('',(0.,-1.,0.));
#17912=DIRECTION('center_axis',(0.,1.,0.));
#17913=DIRECTION('ref_axis',(1.,0.,0.));
#17914=DIRECTION('axis',(0.,0.,1.));
#17915=DIRECTION('refdir',(1.,0.,0.));
#17916=DIRECTION('center_axis',(0.,1.,0.));
#17917=DIRECTION('ref_axis',(1.,0.,0.));
#17918=DIRECTION('center_axis',(0.,1.,0.));
#17919=DIRECTION('ref_axis',(1.,0.,0.));
#17920=DIRECTION('center_axis',(0.,1.,0.));
#17921=DIRECTION('ref_axis',(1.,0.,0.));
#17922=DIRECTION('center_axis',(0.,1.,0.));
#17923=DIRECTION('ref_axis',(1.,0.,0.));
#17924=DIRECTION('',(0.,-1.,0.));
#17925=DIRECTION('center_axis',(0.,1.,0.));
#17926=DIRECTION('ref_axis',(1.,0.,0.));
#17927=DIRECTION('center_axis',(0.,1.,0.));
#17928=DIRECTION('ref_axis',(1.,0.,0.));
#17929=DIRECTION('center_axis',(0.,1.,0.));
#17930=DIRECTION('ref_axis',(1.,0.,0.));
#17931=DIRECTION('center_axis',(0.,1.,0.));
#17932=DIRECTION('ref_axis',(1.,0.,0.));
#17933=DIRECTION('',(0.,-1.,0.));
#17934=DIRECTION('center_axis',(0.,1.,0.));
#17935=DIRECTION('ref_axis',(1.,0.,0.));
#17936=DIRECTION('axis',(0.,0.,1.));
#17937=DIRECTION('refdir',(1.,0.,0.));
#17938=DIRECTION('center_axis',(0.,1.,0.));
#17939=DIRECTION('ref_axis',(1.,0.,0.));
#17940=DIRECTION('center_axis',(0.,1.,0.));
#17941=DIRECTION('ref_axis',(1.,0.,0.));
#17942=DIRECTION('',(0.,1.,0.));
#17943=DIRECTION('center_axis',(0.,-1.,0.));
#17944=DIRECTION('ref_axis',(1.,0.,0.));
#17945=DIRECTION('center_axis',(0.,1.,0.));
#17946=DIRECTION('ref_axis',(1.,0.,0.));
#17947=DIRECTION('center_axis',(0.,1.,0.));
#17948=DIRECTION('ref_axis',(1.,0.,0.));
#17949=DIRECTION('',(0.,1.,0.));
#17950=DIRECTION('center_axis',(0.,-1.,0.));
#17951=DIRECTION('ref_axis',(1.,0.,0.));
#17952=DIRECTION('center_axis',(0.,1.,0.));
#17953=DIRECTION('ref_axis',(1.,0.,0.));
#17954=DIRECTION('center_axis',(0.,1.,0.));
#17955=DIRECTION('ref_axis',(1.,0.,0.));
#17956=DIRECTION('',(0.,1.,0.));
#17957=DIRECTION('center_axis',(0.,-1.,0.));
#17958=DIRECTION('ref_axis',(1.,0.,0.));
#17959=DIRECTION('center_axis',(0.,1.,0.));
#17960=DIRECTION('ref_axis',(1.,0.,0.));
#17961=DIRECTION('center_axis',(0.,1.,0.));
#17962=DIRECTION('ref_axis',(1.,0.,0.));
#17963=DIRECTION('',(0.,1.,0.));
#17964=DIRECTION('center_axis',(0.,-1.,0.));
#17965=DIRECTION('ref_axis',(1.,0.,0.));
#17966=DIRECTION('center_axis',(0.,1.,0.));
#17967=DIRECTION('ref_axis',(1.,0.,0.));
#17968=DIRECTION('center_axis',(0.,-1.,0.));
#17969=DIRECTION('ref_axis',(1.,0.,0.));
#17970=DIRECTION('',(0.,-1.,0.));
#17971=DIRECTION('center_axis',(0.,-1.,0.));
#17972=DIRECTION('ref_axis',(1.,0.,0.));
#17973=DIRECTION('center_axis',(0.,1.,0.));
#17974=DIRECTION('ref_axis',(1.,0.,0.));
#17975=DIRECTION('center_axis',(0.,1.,0.));
#17976=DIRECTION('ref_axis',(1.,0.,0.));
#17977=DIRECTION('',(0.,-1.,0.));
#17978=DIRECTION('center_axis',(0.,1.,0.));
#17979=DIRECTION('ref_axis',(1.,0.,0.));
#17980=DIRECTION('center_axis',(0.,1.,0.));
#17981=DIRECTION('ref_axis',(1.,0.,0.));
#17982=DIRECTION('center_axis',(0.,1.,0.));
#17983=DIRECTION('ref_axis',(1.,0.,0.));
#17984=DIRECTION('axis',(0.,0.,1.));
#17985=DIRECTION('refdir',(1.,0.,0.));
#17986=DIRECTION('center_axis',(0.,1.,0.));
#17987=DIRECTION('ref_axis',(1.,0.,0.));
#17988=DIRECTION('center_axis',(0.,1.,0.));
#17989=DIRECTION('ref_axis',(1.,0.,0.));
#17990=DIRECTION('center_axis',(0.,1.,0.));
#17991=DIRECTION('ref_axis',(1.,0.,0.));
#17992=DIRECTION('center_axis',(0.,1.,0.));
#17993=DIRECTION('ref_axis',(1.,0.,0.));
#17994=DIRECTION('center_axis',(0.,1.,0.));
#17995=DIRECTION('ref_axis',(1.,0.,0.));
#17996=DIRECTION('',(0.,-1.,0.));
#17997=DIRECTION('center_axis',(0.,1.,0.));
#17998=DIRECTION('ref_axis',(1.,0.,0.));
#17999=DIRECTION('center_axis',(0.,1.,0.));
#18000=DIRECTION('ref_axis',(1.,0.,0.));
#18001=DIRECTION('',(0.,-1.,0.));
#18002=DIRECTION('center_axis',(0.,1.,0.));
#18003=DIRECTION('ref_axis',(1.,0.,0.));
#18004=DIRECTION('center_axis',(0.,1.,0.));
#18005=DIRECTION('ref_axis',(1.,0.,0.));
#18006=DIRECTION('axis',(0.,0.,1.));
#18007=DIRECTION('refdir',(1.,0.,0.));
#18008=DIRECTION('center_axis',(0.,1.,0.));
#18009=DIRECTION('ref_axis',(1.,0.,0.));
#18010=DIRECTION('center_axis',(0.,1.,0.));
#18011=DIRECTION('ref_axis',(1.,0.,0.));
#18012=DIRECTION('center_axis',(0.,1.,0.));
#18013=DIRECTION('ref_axis',(1.,0.,0.));
#18014=DIRECTION('center_axis',(0.,1.,0.));
#18015=DIRECTION('ref_axis',(1.,0.,0.));
#18016=DIRECTION('center_axis',(0.,1.,0.));
#18017=DIRECTION('ref_axis',(1.,0.,0.));
#18018=DIRECTION('',(0.,-1.,0.));
#18019=DIRECTION('center_axis',(0.,1.,0.));
#18020=DIRECTION('ref_axis',(1.,0.,0.));
#18021=DIRECTION('center_axis',(0.,1.,0.));
#18022=DIRECTION('ref_axis',(1.,0.,0.));
#18023=DIRECTION('',(0.,-1.,0.));
#18024=DIRECTION('center_axis',(0.,1.,0.));
#18025=DIRECTION('ref_axis',(1.,0.,0.));
#18026=DIRECTION('center_axis',(0.,1.,0.));
#18027=DIRECTION('ref_axis',(1.,0.,0.));
#18028=DIRECTION('axis',(0.,0.,1.));
#18029=DIRECTION('refdir',(1.,0.,0.));
#18030=DIRECTION('center_axis',(0.,1.,0.));
#18031=DIRECTION('ref_axis',(1.,0.,0.));
#18032=DIRECTION('center_axis',(0.,1.,0.));
#18033=DIRECTION('ref_axis',(1.,0.,0.));
#18034=DIRECTION('center_axis',(0.,1.,0.));
#18035=DIRECTION('ref_axis',(1.,0.,0.));
#18036=DIRECTION('center_axis',(0.,1.,0.));
#18037=DIRECTION('ref_axis',(1.,0.,0.));
#18038=DIRECTION('center_axis',(0.,1.,0.));
#18039=DIRECTION('ref_axis',(1.,0.,0.));
#18040=DIRECTION('',(0.,-1.,0.));
#18041=DIRECTION('center_axis',(0.,1.,0.));
#18042=DIRECTION('ref_axis',(1.,0.,0.));
#18043=DIRECTION('center_axis',(0.,1.,0.));
#18044=DIRECTION('ref_axis',(1.,0.,0.));
#18045=DIRECTION('',(0.,-1.,0.));
#18046=DIRECTION('center_axis',(0.,1.,0.));
#18047=DIRECTION('ref_axis',(1.,0.,0.));
#18048=DIRECTION('center_axis',(0.,1.,0.));
#18049=DIRECTION('ref_axis',(1.,0.,0.));
#18050=DIRECTION('axis',(0.,0.,1.));
#18051=DIRECTION('refdir',(1.,0.,0.));
#18052=DIRECTION('center_axis',(0.,1.,0.));
#18053=DIRECTION('ref_axis',(1.,0.,0.));
#18054=DIRECTION('center_axis',(0.,1.,0.));
#18055=DIRECTION('ref_axis',(1.,0.,0.));
#18056=DIRECTION('center_axis',(0.,1.,0.));
#18057=DIRECTION('ref_axis',(1.,0.,0.));
#18058=DIRECTION('center_axis',(0.,1.,0.));
#18059=DIRECTION('ref_axis',(1.,0.,0.));
#18060=DIRECTION('center_axis',(0.,1.,0.));
#18061=DIRECTION('ref_axis',(1.,0.,0.));
#18062=DIRECTION('',(0.,-1.,0.));
#18063=DIRECTION('center_axis',(0.,1.,0.));
#18064=DIRECTION('ref_axis',(1.,0.,0.));
#18065=DIRECTION('center_axis',(0.,1.,0.));
#18066=DIRECTION('ref_axis',(1.,0.,0.));
#18067=DIRECTION('',(0.,-1.,0.));
#18068=DIRECTION('center_axis',(0.,1.,0.));
#18069=DIRECTION('ref_axis',(1.,0.,0.));
#18070=DIRECTION('center_axis',(0.,1.,0.));
#18071=DIRECTION('ref_axis',(1.,0.,0.));
#18072=DIRECTION('axis',(0.,0.,1.));
#18073=DIRECTION('refdir',(1.,0.,0.));
#18074=DIRECTION('axis',(0.,0.,1.));
#18075=DIRECTION('refdir',(1.,0.,0.));
#18076=DIRECTION('center_axis',(0.,-1.,0.));
#18077=DIRECTION('ref_axis',(0.,0.,-1.));
#18078=DIRECTION('center_axis',(0.,-1.,0.));
#18079=DIRECTION('ref_axis',(1.,0.,0.));
#18080=DIRECTION('center_axis',(0.,-1.,0.));
#18081=DIRECTION('ref_axis',(1.,0.,0.));
#18082=DIRECTION('center_axis',(1.,0.,1.22464679914735E-16));
#18083=DIRECTION('ref_axis',(-1.22464679914735E-16,0.,1.));
#18084=DIRECTION('center_axis',(0.,1.,0.));
#18085=DIRECTION('ref_axis',(1.,0.,0.));
#18086=DIRECTION('center_axis',(0.,1.,0.));
#18087=DIRECTION('ref_axis',(1.,0.,0.));
#18088=DIRECTION('center_axis',(0.,-1.,0.));
#18089=DIRECTION('ref_axis',(1.,0.,0.));
#18090=DIRECTION('',(0.,1.,0.));
#18091=DIRECTION('center_axis',(0.,-1.,0.));
#18092=DIRECTION('ref_axis',(1.,0.,0.));
#18093=DIRECTION('center_axis',(0.,-1.,0.));
#18094=DIRECTION('ref_axis',(1.,0.,0.));
#18095=DIRECTION('center_axis',(0.,-1.,0.));
#18096=DIRECTION('ref_axis',(1.,0.,0.));
#18097=DIRECTION('',(0.,1.,0.));
#18098=DIRECTION('center_axis',(0.,-1.,0.));
#18099=DIRECTION('ref_axis',(1.,0.,0.));
#18100=DIRECTION('center_axis',(0.,1.,0.));
#18101=DIRECTION('ref_axis',(1.,0.,0.));
#18102=DIRECTION('',(-0.707106781186548,0.707106781186547,-8.65956056235493E-17));
#18103=DIRECTION('center_axis',(0.,-1.,0.));
#18104=DIRECTION('ref_axis',(1.,0.,0.));
#18105=DIRECTION('center_axis',(0.,1.,0.));
#18106=DIRECTION('ref_axis',(0.,0.,1.));
#18107=DIRECTION('center_axis',(0.,-1.,0.));
#18108=DIRECTION('ref_axis',(1.,0.,0.));
#18109=DIRECTION('center_axis',(0.,-1.,0.));
#18110=DIRECTION('ref_axis',(1.,0.,0.));
#18111=DIRECTION('',(0.,1.,0.));
#18112=DIRECTION('center_axis',(0.,-1.,0.));
#18113=DIRECTION('ref_axis',(0.,0.,-1.));
#18114=DIRECTION('center_axis',(0.,-1.,0.));
#18115=DIRECTION('ref_axis',(1.,0.,0.));
#18116=DIRECTION('center_axis',(0.,-1.,0.));
#18117=DIRECTION('ref_axis',(1.,0.,0.));
#18118=DIRECTION('',(0.707106781186548,0.707106781186547,8.65956056235493E-17));
#18119=DIRECTION('axis',(0.,0.,1.));
#18120=DIRECTION('refdir',(1.,0.,0.));
#18121=DIRECTION('center_axis',(0.,-1.,0.));
#18122=DIRECTION('ref_axis',(0.,0.,-1.));
#18123=DIRECTION('center_axis',(0.,-1.,0.));
#18124=DIRECTION('ref_axis',(1.,0.,0.));
#18125=DIRECTION('center_axis',(0.,-1.,0.));
#18126=DIRECTION('ref_axis',(1.,0.,0.));
#18127=DIRECTION('center_axis',(1.,0.,1.22464679914735E-16));
#18128=DIRECTION('ref_axis',(-1.22464679914735E-16,0.,1.));
#18129=DIRECTION('center_axis',(0.,1.,0.));
#18130=DIRECTION('ref_axis',(1.,0.,0.));
#18131=DIRECTION('center_axis',(0.,1.,0.));
#18132=DIRECTION('ref_axis',(1.,0.,0.));
#18133=DIRECTION('center_axis',(0.,-1.,0.));
#18134=DIRECTION('ref_axis',(1.,0.,0.));
#18135=DIRECTION('center_axis',(0.,-1.,0.));
#18136=DIRECTION('ref_axis',(1.,0.,0.));
#18137=DIRECTION('',(0.,1.,0.));
#18138=DIRECTION('center_axis',(0.,1.,0.));
#18139=DIRECTION('ref_axis',(0.,0.,1.));
#18140=DIRECTION('center_axis',(0.,-1.,0.));
#18141=DIRECTION('ref_axis',(1.,0.,0.));
#18142=DIRECTION('center_axis',(0.,-1.,0.));
#18143=DIRECTION('ref_axis',(1.,0.,0.));
#18144=DIRECTION('center_axis',(0.,-1.,0.));
#18145=DIRECTION('ref_axis',(1.,0.,0.));
#18146=DIRECTION('center_axis',(0.,-1.,0.));
#18147=DIRECTION('ref_axis',(1.,0.,0.));
#18148=DIRECTION('',(0.707106781186548,0.707106781186547,8.65956056235494E-17));
#18149=DIRECTION('center_axis',(0.,-1.,0.));
#18150=DIRECTION('ref_axis',(1.,0.,0.));
#18151=DIRECTION('center_axis',(0.,-1.,0.));
#18152=DIRECTION('ref_axis',(1.,0.,0.));
#18153=DIRECTION('',(0.,1.,0.));
#18154=DIRECTION('center_axis',(0.,1.,0.));
#18155=DIRECTION('ref_axis',(1.,0.,0.));
#18156=DIRECTION('center_axis',(0.,-1.,0.));
#18157=DIRECTION('ref_axis',(1.,0.,0.));
#18158=DIRECTION('',(-0.707106781186548,0.707106781186547,-8.65956056235494E-17));
#18159=DIRECTION('center_axis',(0.,-1.,0.));
#18160=DIRECTION('ref_axis',(0.,0.,-1.));
#18161=DIRECTION('center_axis',(0.,-1.,0.));
#18162=DIRECTION('ref_axis',(1.,0.,0.));
#18163=DIRECTION('',(0.,1.,0.));
#18164=DIRECTION('axis',(0.,0.,1.));
#18165=DIRECTION('refdir',(1.,0.,0.));
#18166=DIRECTION('center_axis',(0.,0.,1.));
#18167=DIRECTION('ref_axis',(1.,0.,0.));
#18168=DIRECTION('center_axis',(1.22464679914735E-16,-1.,0.));
#18169=DIRECTION('ref_axis',(-1.,-1.22464679914735E-16,0.));
#18170=DIRECTION('center_axis',(0.78183148246803,0.,0.623489801858733));
#18171=DIRECTION('ref_axis',(0.623489801858734,0.,-0.78183148246803));
#18172=DIRECTION('center_axis',(7.63554790147315E-17,-1.,-9.57467422477103E-17));
#18173=DIRECTION('ref_axis',(-0.623489801858734,-1.22464679914735E-16,0.78183148246803));
#18174=DIRECTION('center_axis',(0.974927912181824,0.,-0.222520933956314));
#18175=DIRECTION('ref_axis',(-0.222520933956314,0.,-0.974927912181824));
#18176=DIRECTION('center_axis',(-2.7250954951288E-17,-1.,-1.19394234705288E-16));
#18177=DIRECTION('ref_axis',(0.222520933956314,-1.22464679914735E-16,0.974927912181824));
#18178=DIRECTION('center_axis',(0.433883739117558,0.,-0.900968867902419));
#18179=DIRECTION('ref_axis',(-0.900968867902419,0.,-0.433883739117558));
#18180=DIRECTION('center_axis',(-1.10336864020811E-16,-1.,-5.31354332312403E-17));
#18181=DIRECTION('ref_axis',(0.900968867902419,-1.22464679914735E-16,0.433883739117558));
#18182=DIRECTION('center_axis',(-0.433883739117558,0.,-0.900968867902419));
#18183=DIRECTION('ref_axis',(-0.900968867902419,0.,0.433883739117558));
#18184=DIRECTION('center_axis',(-1.10336864020811E-16,-1.,5.31354332312403E-17));
#18185=DIRECTION('ref_axis',(0.900968867902419,-1.22464679914735E-16,-0.433883739117558));
#18186=DIRECTION('center_axis',(-0.974927912181824,0.,-0.222520933956314));
#18187=DIRECTION('ref_axis',(-0.222520933956315,0.,0.974927912181824));
#18188=DIRECTION('center_axis',(-2.7250954951288E-17,-1.,1.19394234705288E-16));
#18189=DIRECTION('ref_axis',(0.222520933956315,-1.22464679914735E-16,-0.974927912181824));
#18190=DIRECTION('center_axis',(-0.78183148246803,0.,0.623489801858734));
#18191=DIRECTION('ref_axis',(0.623489801858733,0.,0.78183148246803));
#18192=DIRECTION('center_axis',(7.63554790147315E-17,-1.,9.57467422477103E-17));
#18193=DIRECTION('ref_axis',(-0.623489801858733,-1.22464679914735E-16,-0.78183148246803));
#18194=DIRECTION('axis',(0.,0.,1.));
#18195=DIRECTION('refdir',(1.,0.,0.));
#18196=DIRECTION('center_axis',(0.,0.,1.));
#18197=DIRECTION('ref_axis',(1.,0.,0.));
#18198=DIRECTION('center_axis',(0.,-1.,0.));
#18199=DIRECTION('ref_axis',(0.,0.,-1.));
#18200=DIRECTION('center_axis',(0.,-1.,0.));
#18201=DIRECTION('ref_axis',(0.,0.,-1.));
#18202=DIRECTION('center_axis',(0.,1.,0.));
#18203=DIRECTION('ref_axis',(1.,0.,0.));
#18204=DIRECTION('center_axis',(0.,1.,0.));
#18205=DIRECTION('ref_axis',(1.,0.,0.));
#18206=DIRECTION('center_axis',(0.,1.,0.));
#18207=DIRECTION('ref_axis',(1.,0.,0.));
#18208=DIRECTION('center_axis',(0.,1.,0.));
#18209=DIRECTION('ref_axis',(1.,0.,0.));
#18210=DIRECTION('',(0.,-1.,0.));
#18211=DIRECTION('center_axis',(0.,-1.,0.));
#18212=DIRECTION('ref_axis',(1.,0.,0.));
#18213=DIRECTION('center_axis',(0.,1.,0.));
#18214=DIRECTION('ref_axis',(1.,0.,0.));
#18215=DIRECTION('center_axis',(0.,1.,0.));
#18216=DIRECTION('ref_axis',(1.,0.,0.));
#18217=DIRECTION('center_axis',(0.,1.,0.));
#18218=DIRECTION('ref_axis',(1.,0.,0.));
#18219=DIRECTION('center_axis',(0.,1.,0.));
#18220=DIRECTION('ref_axis',(1.,0.,0.));
#18221=DIRECTION('center_axis',(0.,1.,0.));
#18222=DIRECTION('ref_axis',(1.,0.,0.));
#18223=DIRECTION('center_axis',(0.,1.,0.));
#18224=DIRECTION('ref_axis',(1.,0.,0.));
#18225=DIRECTION('center_axis',(0.,-1.,0.));
#18226=DIRECTION('ref_axis',(1.,0.,0.));
#18227=DIRECTION('center_axis',(0.,-1.,0.));
#18228=DIRECTION('ref_axis',(0.,0.,-1.));
#18229=DIRECTION('center_axis',(8.96625347776458E-17,0.,1.));
#18230=DIRECTION('ref_axis',(1.,0.,0.));
#18231=DIRECTION('center_axis',(0.,-1.,0.));
#18232=DIRECTION('ref_axis',(0.,0.,-1.));
#18233=DIRECTION('center_axis',(0.,1.,0.));
#18234=DIRECTION('ref_axis',(1.,0.,0.));
#18235=DIRECTION('center_axis',(0.,-1.,0.));
#18236=DIRECTION('ref_axis',(1.,0.,0.));
#18237=DIRECTION('center_axis',(0.,-1.,0.));
#18238=DIRECTION('ref_axis',(0.,0.,-1.));
#18239=DIRECTION('center_axis',(0.,0.,1.));
#18240=DIRECTION('ref_axis',(1.,0.,0.));
#18241=DIRECTION('center_axis',(0.,-1.,0.));
#18242=DIRECTION('ref_axis',(0.,0.,-1.));
#18243=DIRECTION('center_axis',(0.,1.,0.));
#18244=DIRECTION('ref_axis',(1.,0.,0.));
#18245=DIRECTION('center_axis',(0.,-1.,0.));
#18246=DIRECTION('ref_axis',(1.,0.,0.));
#18247=DIRECTION('center_axis',(0.,-1.,0.));
#18248=DIRECTION('ref_axis',(1.,0.,0.));
#18249=DIRECTION('center_axis',(0.,-1.,0.));
#18250=DIRECTION('ref_axis',(0.,0.,-1.));
#18251=DIRECTION('center_axis',(0.,0.,1.));
#18252=DIRECTION('ref_axis',(1.,0.,0.));
#18253=DIRECTION('center_axis',(0.,-1.,0.));
#18254=DIRECTION('ref_axis',(0.,0.,-1.));
#18255=DIRECTION('center_axis',(0.,1.,0.));
#18256=DIRECTION('ref_axis',(1.,0.,0.));
#18257=DIRECTION('center_axis',(0.,-1.,0.));
#18258=DIRECTION('ref_axis',(1.,0.,0.));
#18259=DIRECTION('center_axis',(0.,-1.,0.));
#18260=DIRECTION('ref_axis',(0.,0.,-1.));
#18261=DIRECTION('center_axis',(8.96625347776458E-17,0.,1.));
#18262=DIRECTION('ref_axis',(1.,0.,0.));
#18263=DIRECTION('center_axis',(0.,-1.,0.));
#18264=DIRECTION('ref_axis',(0.,0.,-1.));
#18265=DIRECTION('center_axis',(0.,1.,0.));
#18266=DIRECTION('ref_axis',(1.,0.,0.));
#18267=DIRECTION('center_axis',(0.,-1.,0.));
#18268=DIRECTION('ref_axis',(1.,0.,0.));
#18269=DIRECTION('center_axis',(0.,-1.,0.));
#18270=DIRECTION('ref_axis',(0.,0.,-1.));
#18271=DIRECTION('center_axis',(0.,0.,1.));
#18272=DIRECTION('ref_axis',(1.,0.,0.));
#18273=DIRECTION('center_axis',(0.,-1.,0.));
#18274=DIRECTION('ref_axis',(0.,0.,-1.));
#18275=DIRECTION('center_axis',(0.,1.,0.));
#18276=DIRECTION('ref_axis',(1.,0.,0.));
#18277=DIRECTION('center_axis',(0.,1.,0.));
#18278=DIRECTION('ref_axis',(1.,0.,0.));
#18279=DIRECTION('',(0.,1.,0.));
#18280=DIRECTION('center_axis',(0.,-1.,0.));
#18281=DIRECTION('ref_axis',(1.,0.,0.));
#18282=DIRECTION('center_axis',(0.,-1.,0.));
#18283=DIRECTION('ref_axis',(1.,0.,0.));
#18284=DIRECTION('center_axis',(0.,1.,0.));
#18285=DIRECTION('ref_axis',(1.,0.,0.));
#18286=DIRECTION('center_axis',(0.,-1.,0.));
#18287=DIRECTION('ref_axis',(0.,0.,-1.));
#18288=DIRECTION('center_axis',(0.,0.,1.));
#18289=DIRECTION('ref_axis',(1.,0.,0.));
#18290=DIRECTION('center_axis',(0.,-1.,0.));
#18291=DIRECTION('ref_axis',(0.,0.,-1.));
#18292=DIRECTION('center_axis',(0.,-1.,0.));
#18293=DIRECTION('ref_axis',(-1.,0.,0.));
#18294=DIRECTION('center_axis',(0.,1.,0.));
#18295=DIRECTION('ref_axis',(1.,0.,0.));
#18296=DIRECTION('axis',(0.,0.,1.));
#18297=DIRECTION('refdir',(1.,0.,0.));
#18298=DIRECTION('center_axis',(0.,1.,0.));
#18299=DIRECTION('ref_axis',(0.,0.,1.));
#18300=DIRECTION('center_axis',(0.,-1.,0.));
#18301=DIRECTION('ref_axis',(1.,0.,0.));
#18302=DIRECTION('center_axis',(0.,-1.,0.));
#18303=DIRECTION('ref_axis',(1.,0.,0.));
#18304=DIRECTION('center_axis',(0.,-1.,0.));
#18305=DIRECTION('ref_axis',(1.,0.,0.));
#18306=DIRECTION('center_axis',(0.,-1.,0.));
#18307=DIRECTION('ref_axis',(1.,0.,0.));
#18308=DIRECTION('',(0.,1.,0.));
#18309=DIRECTION('center_axis',(0.,-1.,0.));
#18310=DIRECTION('ref_axis',(0.,0.,-1.));
#18311=DIRECTION('center_axis',(0.,-1.,0.));
#18312=DIRECTION('ref_axis',(1.,0.,0.));
#18313=DIRECTION('center_axis',(0.,-1.,0.));
#18314=DIRECTION('ref_axis',(1.,0.,0.));
#18315=DIRECTION('',(0.,1.,0.));
#18316=DIRECTION('center_axis',(0.,1.,0.));
#18317=DIRECTION('ref_axis',(0.,0.,1.));
#18318=DIRECTION('center_axis',(0.,-1.,0.));
#18319=DIRECTION('ref_axis',(1.,0.,0.));
#18320=DIRECTION('center_axis',(0.,-1.,0.));
#18321=DIRECTION('ref_axis',(1.,0.,0.));
#18322=DIRECTION('center_axis',(0.,-1.,0.));
#18323=DIRECTION('ref_axis',(1.,0.,0.));
#18324=DIRECTION('center_axis',(0.,-1.,0.));
#18325=DIRECTION('ref_axis',(1.,0.,0.));
#18326=DIRECTION('',(0.,1.,0.));
#18327=DIRECTION('center_axis',(0.,-1.,0.));
#18328=DIRECTION('ref_axis',(0.,0.,-1.));
#18329=DIRECTION('center_axis',(0.,-1.,0.));
#18330=DIRECTION('ref_axis',(1.,0.,0.));
#18331=DIRECTION('center_axis',(0.,-1.,0.));
#18332=DIRECTION('ref_axis',(1.,0.,0.));
#18333=DIRECTION('',(0.,1.,0.));
#18334=DIRECTION('',(0.,0.,1.));
#18335=DIRECTION('',(1.,0.,0.));
#18336=DIRECTION('',(0.,0.,1.));
#18337=DIRECTION('',(1.,0.,0.));
#18338=DIRECTION('',(0.,0.,1.));
#18339=DIRECTION('',(1.,0.,0.));
#18340=DIRECTION('',(0.,0.,1.));
#18341=DIRECTION('',(1.,0.,0.));
#18342=DIRECTION('',(0.,0.,1.));
#18343=DIRECTION('',(1.,0.,0.));
#18344=DIRECTION('',(0.,0.,1.));
#18345=DIRECTION('',(1.,0.,0.));
#18346=DIRECTION('',(0.,0.,1.));
#18347=DIRECTION('',(1.,0.,0.));
#18348=DIRECTION('',(0.,0.,1.));
#18349=DIRECTION('',(1.,0.,0.));
#18350=DIRECTION('',(0.,0.,1.));
#18351=DIRECTION('',(1.,0.,0.));
#18352=DIRECTION('',(0.,0.,1.));
#18353=DIRECTION('',(1.,0.,0.));
#18354=DIRECTION('',(0.,0.,1.));
#18355=DIRECTION('',(1.,0.,0.));
#18356=DIRECTION('',(0.,0.,1.));
#18357=DIRECTION('',(1.,0.,0.));
#18358=DIRECTION('',(0.,0.,1.));
#18359=DIRECTION('',(1.,0.,0.));
#18360=DIRECTION('',(0.,0.,1.));
#18361=DIRECTION('',(1.,0.,0.));
#18362=DIRECTION('',(0.,0.,1.));
#18363=DIRECTION('',(1.,0.,0.));
#18364=DIRECTION('',(0.,0.,1.));
#18365=DIRECTION('',(1.,0.,0.));
#18366=DIRECTION('',(0.,0.,1.));
#18367=DIRECTION('',(1.,0.,0.));
#18368=DIRECTION('',(0.,0.,1.));
#18369=DIRECTION('',(1.,0.,0.));
#18370=DIRECTION('',(0.,0.,1.));
#18371=DIRECTION('',(1.,0.,0.));
#18372=DIRECTION('',(0.,0.,1.));
#18373=DIRECTION('',(1.,0.,0.));
#18374=DIRECTION('',(0.,0.,1.));
#18375=DIRECTION('',(1.,0.,0.));
#18376=DIRECTION('',(0.,0.,1.));
#18377=DIRECTION('',(1.,0.,0.));
#18378=DIRECTION('',(0.,0.,1.));
#18379=DIRECTION('',(1.,0.,0.));
#18380=DIRECTION('',(0.,0.,1.));
#18381=DIRECTION('',(1.,0.,0.));
#18382=DIRECTION('',(0.,0.,1.));
#18383=DIRECTION('',(1.,0.,0.));
#18384=DIRECTION('',(0.,0.,1.));
#18385=DIRECTION('',(1.,0.,0.));
#18386=DIRECTION('',(0.,0.,1.));
#18387=DIRECTION('',(1.,0.,0.));
#18388=DIRECTION('',(0.,0.,1.));
#18389=DIRECTION('',(1.,0.,0.));
#18390=DIRECTION('',(0.,0.,1.));
#18391=DIRECTION('',(1.,0.,0.));
#18392=DIRECTION('',(0.,0.,1.));
#18393=DIRECTION('',(1.,0.,0.));
#18394=DIRECTION('',(0.,0.,1.));
#18395=DIRECTION('',(1.,0.,0.));
#18396=DIRECTION('',(0.,0.,1.));
#18397=DIRECTION('',(1.,0.,0.));
#18398=DIRECTION('',(0.,0.,1.));
#18399=DIRECTION('',(1.,0.,0.));
#18400=DIRECTION('',(0.,0.,1.));
#18401=DIRECTION('',(1.,0.,0.));
#18402=DIRECTION('',(0.,0.,1.));
#18403=DIRECTION('',(1.,0.,0.));
#18404=DIRECTION('',(0.,0.,1.));
#18405=DIRECTION('',(1.,0.,0.));
#18406=DIRECTION('',(0.,0.,1.));
#18407=DIRECTION('',(1.,0.,0.));
#18408=DIRECTION('',(0.,0.,1.));
#18409=DIRECTION('',(1.,0.,0.));
#18410=DIRECTION('',(0.,0.,1.));
#18411=DIRECTION('',(1.,0.,0.));
#18412=DIRECTION('',(0.,0.,1.));
#18413=DIRECTION('',(1.,0.,0.));
#18414=DIRECTION('',(0.,0.,1.));
#18415=DIRECTION('',(1.,0.,0.));
#18416=DIRECTION('',(0.,0.,1.));
#18417=DIRECTION('',(1.,0.,0.));
#18418=DIRECTION('',(0.,0.,1.));
#18419=DIRECTION('',(1.,0.,0.));
#18420=DIRECTION('',(0.,0.,1.));
#18421=DIRECTION('',(1.,0.,0.));
#18422=DIRECTION('',(0.,0.,1.));
#18423=DIRECTION('',(1.,0.,0.));
#18424=DIRECTION('',(0.,0.,1.));
#18425=DIRECTION('',(1.,0.,0.));
#18426=DIRECTION('',(0.,0.,1.));
#18427=DIRECTION('',(1.,0.,0.));
#18428=DIRECTION('',(0.,0.,1.));
#18429=DIRECTION('',(1.,0.,0.));
#18430=DIRECTION('',(0.,0.,1.));
#18431=DIRECTION('',(1.,0.,0.));
#18432=DIRECTION('',(0.,0.,1.));
#18433=DIRECTION('',(1.,0.,0.));
#18434=DIRECTION('',(0.,0.,1.));
#18435=DIRECTION('',(1.,0.,0.));
#18436=DIRECTION('axis',(0.,0.,1.));
#18437=DIRECTION('refdir',(1.,0.,0.));
#18438=DIRECTION('axis',(0.,0.,1.));
#18439=DIRECTION('refdir',(1.,0.,0.));
#18440=DIRECTION('center_axis',(0.,1.,0.));
#18441=DIRECTION('ref_axis',(1.,0.,0.));
#18442=DIRECTION('center_axis',(0.,1.,0.));
#18443=DIRECTION('ref_axis',(1.,0.,0.));
#18444=DIRECTION('',(0.,1.,0.));
#18445=DIRECTION('center_axis',(0.,-1.,0.));
#18446=DIRECTION('ref_axis',(1.,0.,0.));
#18447=DIRECTION('center_axis',(0.,1.,0.));
#18448=DIRECTION('ref_axis',(1.,0.,0.));
#18449=DIRECTION('center_axis',(0.,1.,0.));
#18450=DIRECTION('ref_axis',(1.,0.,0.));
#18451=DIRECTION('',(0.,1.,0.));
#18452=DIRECTION('center_axis',(0.,-1.,0.));
#18453=DIRECTION('ref_axis',(1.,0.,0.));
#18454=DIRECTION('center_axis',(0.,1.,0.));
#18455=DIRECTION('ref_axis',(1.,0.,0.));
#18456=DIRECTION('center_axis',(0.,1.,0.));
#18457=DIRECTION('ref_axis',(1.,0.,0.));
#18458=DIRECTION('',(0.,1.,0.));
#18459=DIRECTION('center_axis',(0.,-1.,0.));
#18460=DIRECTION('ref_axis',(1.,0.,0.));
#18461=DIRECTION('center_axis',(0.,1.,0.));
#18462=DIRECTION('ref_axis',(1.,0.,0.));
#18463=DIRECTION('center_axis',(0.,1.,0.));
#18464=DIRECTION('ref_axis',(1.,0.,0.));
#18465=DIRECTION('',(0.,1.,0.));
#18466=DIRECTION('center_axis',(0.,-1.,0.));
#18467=DIRECTION('ref_axis',(1.,0.,0.));
#18468=DIRECTION('center_axis',(0.,1.,0.));
#18469=DIRECTION('ref_axis',(1.,0.,0.));
#18470=DIRECTION('center_axis',(0.,1.,0.));
#18471=DIRECTION('ref_axis',(1.,0.,0.));
#18472=DIRECTION('',(0.,1.,0.));
#18473=DIRECTION('center_axis',(0.,-1.,0.));
#18474=DIRECTION('ref_axis',(1.,0.,0.));
#18475=DIRECTION('center_axis',(0.,1.,0.));
#18476=DIRECTION('ref_axis',(1.,0.,0.));
#18477=DIRECTION('center_axis',(0.,1.,0.));
#18478=DIRECTION('ref_axis',(1.,0.,0.));
#18479=DIRECTION('',(0.,1.,0.));
#18480=DIRECTION('center_axis',(0.,-1.,0.));
#18481=DIRECTION('ref_axis',(1.,0.,0.));
#18482=DIRECTION('center_axis',(0.,1.,0.));
#18483=DIRECTION('ref_axis',(1.,0.,0.));
#18484=DIRECTION('center_axis',(0.,1.,0.));
#18485=DIRECTION('ref_axis',(1.,0.,0.));
#18486=DIRECTION('',(0.,1.,0.));
#18487=DIRECTION('center_axis',(0.,-1.,0.));
#18488=DIRECTION('ref_axis',(1.,0.,0.));
#18489=DIRECTION('center_axis',(0.,1.,0.));
#18490=DIRECTION('ref_axis',(1.,0.,0.));
#18491=DIRECTION('center_axis',(0.,1.,0.));
#18492=DIRECTION('ref_axis',(1.,0.,0.));
#18493=DIRECTION('',(0.,1.,0.));
#18494=DIRECTION('center_axis',(0.,-1.,0.));
#18495=DIRECTION('ref_axis',(1.,0.,0.));
#18496=DIRECTION('center_axis',(-1.,0.,0.));
#18497=DIRECTION('ref_axis',(0.,0.,1.));
#18498=DIRECTION('',(0.,1.,0.));
#18499=DIRECTION('',(0.,0.,-1.));
#18500=DIRECTION('',(0.,1.,0.));
#18501=DIRECTION('',(0.,0.,1.));
#18502=DIRECTION('center_axis',(1.,0.,0.));
#18503=DIRECTION('ref_axis',(0.,0.,-1.));
#18504=DIRECTION('',(0.,-1.,0.));
#18505=DIRECTION('',(0.,0.,-1.));
#18506=DIRECTION('',(0.,1.,0.));
#18507=DIRECTION('',(0.,0.,1.));
#18508=DIRECTION('center_axis',(0.,0.,1.));
#18509=DIRECTION('ref_axis',(1.,0.,0.));
#18510=DIRECTION('',(-1.,0.,0.));
#18511=DIRECTION('',(1.,0.,0.));
#18512=DIRECTION('center_axis',(0.,1.,0.));
#18513=DIRECTION('ref_axis',(1.,0.,0.));
#18514=DIRECTION('center_axis',(0.,1.,0.));
#18515=DIRECTION('ref_axis',(1.,0.,0.));
#18516=DIRECTION('',(0.,1.,0.));
#18517=DIRECTION('center_axis',(0.,1.,0.));
#18518=DIRECTION('ref_axis',(1.,0.,0.));
#18519=DIRECTION('center_axis',(0.,1.,0.));
#18520=DIRECTION('ref_axis',(1.,0.,0.));
#18521=DIRECTION('center_axis',(0.,1.,0.));
#18522=DIRECTION('ref_axis',(1.,0.,0.));
#18523=DIRECTION('',(0.,-1.,0.));
#18524=DIRECTION('center_axis',(0.,1.,0.));
#18525=DIRECTION('ref_axis',(1.,0.,0.));
#18526=DIRECTION('center_axis',(0.,1.,0.));
#18527=DIRECTION('ref_axis',(1.,0.,0.));
#18528=DIRECTION('',(0.822508459509058,0.,0.568752876068364));
#18529=DIRECTION('',(0.,0.,1.));
#18530=DIRECTION('',(-1.,0.,0.));
#18531=DIRECTION('',(0.,0.,-1.));
#18532=DIRECTION('center_axis',(0.,1.,0.));
#18533=DIRECTION('ref_axis',(1.,0.,0.));
#18534=DIRECTION('',(-0.822508459509058,0.,-0.568752876068364));
#18535=DIRECTION('center_axis',(-1.,0.,0.));
#18536=DIRECTION('ref_axis',(0.,0.,1.));
#18537=DIRECTION('',(0.,1.,0.));
#18538=DIRECTION('',(0.,1.,0.));
#18539=DIRECTION('',(0.,0.,1.));
#18540=DIRECTION('center_axis',(1.,0.,0.));
#18541=DIRECTION('ref_axis',(0.,0.,-1.));
#18542=DIRECTION('',(0.,-1.,0.));
#18543=DIRECTION('',(0.,0.,-1.));
#18544=DIRECTION('',(0.,1.,0.));
#18545=DIRECTION('center_axis',(0.,0.,1.));
#18546=DIRECTION('ref_axis',(1.,0.,0.));
#18547=DIRECTION('',(1.,0.,0.));
#18548=DIRECTION('center_axis',(-0.568752876068364,0.,0.822508459509058));
#18549=DIRECTION('ref_axis',(0.822508459509058,0.,0.568752876068364));
#18550=DIRECTION('',(0.822508459509058,0.,0.568752876068364));
#18551=DIRECTION('center_axis',(0.,1.,0.));
#18552=DIRECTION('ref_axis',(-0.432056364839205,0.,-0.901846604252592));
#18553=DIRECTION('center_axis',(0.,1.,0.));
#18554=DIRECTION('ref_axis',(1.,0.,0.));
#18555=DIRECTION('',(0.,1.,0.));
#18556=DIRECTION('center_axis',(0.568752876068364,0.,-0.822508459509058));
#18557=DIRECTION('ref_axis',(-0.822508459509058,0.,-0.568752876068364));
#18558=DIRECTION('',(-0.822508459509058,0.,-0.568752876068364));
#18559=DIRECTION('center_axis',(0.,1.,0.));
#18560=DIRECTION('ref_axis',(0.,0.,1.));
#18561=DIRECTION('center_axis',(0.,1.,0.));
#18562=DIRECTION('ref_axis',(-1.,0.,0.));
#18563=DIRECTION('',(-1.,0.,0.));
#18564=DIRECTION('',(0.,0.,1.));
#18565=DIRECTION('',(-1.,0.,0.));
#18566=DIRECTION('',(0.,0.,1.));
#18567=DIRECTION('center_axis',(1.,0.,0.));
#18568=DIRECTION('ref_axis',(0.,1.,0.));
#18569=DIRECTION('',(0.,1.,0.));
#18570=DIRECTION('',(0.,1.,0.));
#18571=DIRECTION('',(0.,0.,1.));
#18572=DIRECTION('center_axis',(0.,-1.,0.));
#18573=DIRECTION('ref_axis',(1.,0.,0.));
#18574=DIRECTION('',(1.,0.,0.));
#18575=DIRECTION('',(1.,0.,0.));
#18576=DIRECTION('',(0.,0.,1.));
#18577=DIRECTION('center_axis',(-1.,0.,0.));
#18578=DIRECTION('ref_axis',(0.,-1.,0.));
#18579=DIRECTION('',(0.,-1.,0.));
#18580=DIRECTION('',(0.,-1.,0.));
#18581=DIRECTION('center_axis',(0.,0.,1.));
#18582=DIRECTION('ref_axis',(1.,0.,0.));
#18583=DIRECTION('center_axis',(0.,0.,1.));
#18584=DIRECTION('ref_axis',(1.,0.,0.));
#18585=DIRECTION('axis',(0.,0.,1.));
#18586=DIRECTION('refdir',(1.,0.,0.));
#18587=DIRECTION('center_axis',(0.,1.,0.));
#18588=DIRECTION('ref_axis',(-1.,0.,0.));
#18589=DIRECTION('',(-1.,0.,0.));
#18590=DIRECTION('',(0.,0.,1.));
#18591=DIRECTION('',(-1.,0.,0.));
#18592=DIRECTION('',(0.,0.,1.));
#18593=DIRECTION('center_axis',(1.,0.,0.));
#18594=DIRECTION('ref_axis',(0.,1.,0.));
#18595=DIRECTION('',(0.,1.,0.));
#18596=DIRECTION('',(0.,1.,0.));
#18597=DIRECTION('',(0.,0.,1.));
#18598=DIRECTION('center_axis',(0.,-1.,0.));
#18599=DIRECTION('ref_axis',(1.,0.,0.));
#18600=DIRECTION('',(1.,0.,0.));
#18601=DIRECTION('',(1.,0.,0.));
#18602=DIRECTION('',(0.,0.,1.));
#18603=DIRECTION('center_axis',(-1.,0.,0.));
#18604=DIRECTION('ref_axis',(0.,-1.,0.));
#18605=DIRECTION('',(0.,-1.,0.));
#18606=DIRECTION('',(0.,-1.,0.));
#18607=DIRECTION('center_axis',(0.,0.,1.));
#18608=DIRECTION('ref_axis',(1.,0.,0.));
#18609=DIRECTION('center_axis',(0.,0.,1.));
#18610=DIRECTION('ref_axis',(1.,0.,0.));
#18611=DIRECTION('axis',(0.,0.,1.));
#18612=DIRECTION('refdir',(1.,0.,0.));
#18613=DIRECTION('center_axis',(0.,1.,0.));
#18614=DIRECTION('ref_axis',(-1.,0.,0.));
#18615=DIRECTION('',(-1.,0.,0.));
#18616=DIRECTION('',(0.,0.,1.));
#18617=DIRECTION('',(-1.,0.,0.));
#18618=DIRECTION('',(0.,0.,1.));
#18619=DIRECTION('center_axis',(1.,0.,0.));
#18620=DIRECTION('ref_axis',(0.,1.,0.));
#18621=DIRECTION('',(0.,1.,0.));
#18622=DIRECTION('',(0.,1.,0.));
#18623=DIRECTION('',(0.,0.,1.));
#18624=DIRECTION('center_axis',(0.,-1.,0.));
#18625=DIRECTION('ref_axis',(1.,0.,0.));
#18626=DIRECTION('',(1.,0.,0.));
#18627=DIRECTION('',(1.,0.,0.));
#18628=DIRECTION('',(0.,0.,1.));
#18629=DIRECTION('center_axis',(-1.,0.,0.));
#18630=DIRECTION('ref_axis',(0.,-1.,0.));
#18631=DIRECTION('',(0.,-1.,0.));
#18632=DIRECTION('',(0.,-1.,0.));
#18633=DIRECTION('center_axis',(0.,0.,1.));
#18634=DIRECTION('ref_axis',(1.,0.,0.));
#18635=DIRECTION('center_axis',(0.,0.,1.));
#18636=DIRECTION('ref_axis',(1.,0.,0.));
#18637=DIRECTION('axis',(0.,0.,1.));
#18638=DIRECTION('refdir',(1.,0.,0.));
#18639=DIRECTION('center_axis',(0.,1.,0.));
#18640=DIRECTION('ref_axis',(1.,0.,0.));
#18641=DIRECTION('center_axis',(0.,1.,0.));
#18642=DIRECTION('ref_axis',(1.,0.,0.));
#18643=DIRECTION('',(0.,1.,0.));
#18644=DIRECTION('center_axis',(0.,1.,0.));
#18645=DIRECTION('ref_axis',(1.,0.,0.));
#18646=DIRECTION('center_axis',(0.,1.,0.));
#18647=DIRECTION('ref_axis',(1.,0.,0.));
#18648=DIRECTION('center_axis',(0.,1.,0.));
#18649=DIRECTION('ref_axis',(1.,0.,0.));
#18650=DIRECTION('center_axis',(0.,1.,0.));
#18651=DIRECTION('ref_axis',(1.,0.,0.));
#18652=DIRECTION('',(0.,1.,0.));
#18653=DIRECTION('center_axis',(0.,-1.,0.));
#18654=DIRECTION('ref_axis',(1.,0.,0.));
#18655=DIRECTION('center_axis',(0.,1.,0.));
#18656=DIRECTION('ref_axis',(1.,0.,0.));
#18657=DIRECTION('center_axis',(0.,1.,0.));
#18658=DIRECTION('ref_axis',(1.,0.,0.));
#18659=DIRECTION('',(0.,1.,0.));
#18660=DIRECTION('center_axis',(0.,-1.,0.));
#18661=DIRECTION('ref_axis',(1.,0.,0.));
#18662=DIRECTION('center_axis',(0.,1.,0.));
#18663=DIRECTION('ref_axis',(1.,0.,0.));
#18664=DIRECTION('center_axis',(0.,1.,0.));
#18665=DIRECTION('ref_axis',(1.,0.,0.));
#18666=DIRECTION('',(0.,1.,0.));
#18667=DIRECTION('center_axis',(0.,-1.,0.));
#18668=DIRECTION('ref_axis',(1.,0.,0.));
#18669=DIRECTION('center_axis',(0.,1.,0.));
#18670=DIRECTION('ref_axis',(1.,0.,0.));
#18671=DIRECTION('center_axis',(0.,1.,0.));
#18672=DIRECTION('ref_axis',(1.,0.,0.));
#18673=DIRECTION('center_axis',(0.,1.,0.));
#18674=DIRECTION('ref_axis',(1.,0.,0.));
#18675=DIRECTION('center_axis',(0.,1.,0.));
#18676=DIRECTION('ref_axis',(1.,0.,0.));
#18677=DIRECTION('center_axis',(0.,1.,0.));
#18678=DIRECTION('ref_axis',(1.,0.,0.));
#18679=DIRECTION('center_axis',(0.,-1.,0.));
#18680=DIRECTION('ref_axis',(1.,0.,0.));
#18681=DIRECTION('center_axis',(0.,1.,0.));
#18682=DIRECTION('ref_axis',(1.,0.,0.));
#18683=DIRECTION('',(0.,-1.,0.));
#18684=DIRECTION('center_axis',(0.,1.,0.));
#18685=DIRECTION('ref_axis',(1.,0.,0.));
#18686=DIRECTION('',(0.,-1.,0.));
#18687=DIRECTION('center_axis',(0.,1.,0.));
#18688=DIRECTION('ref_axis',(1.,0.,0.));
#18689=DIRECTION('center_axis',(0.,1.,0.));
#18690=DIRECTION('ref_axis',(1.,0.,0.));
#18691=DIRECTION('center_axis',(0.,1.,0.));
#18692=DIRECTION('ref_axis',(1.,0.,0.));
#18693=DIRECTION('',(0.,-1.,0.));
#18694=DIRECTION('center_axis',(0.,1.,0.));
#18695=DIRECTION('ref_axis',(1.,0.,0.));
#18696=DIRECTION('center_axis',(0.,1.,0.));
#18697=DIRECTION('ref_axis',(1.,0.,0.));
#18698=DIRECTION('axis',(0.,0.,1.));
#18699=DIRECTION('refdir',(1.,0.,0.));
#18700=DIRECTION('center_axis',(0.,1.,0.));
#18701=DIRECTION('ref_axis',(1.,0.,0.));
#18702=DIRECTION('center_axis',(0.,-1.,0.));
#18703=DIRECTION('ref_axis',(1.,0.,0.));
#18704=DIRECTION('',(0.,-1.,0.));
#18705=DIRECTION('center_axis',(0.,-1.,0.));
#18706=DIRECTION('ref_axis',(1.,0.,0.));
#18707=DIRECTION('center_axis',(0.,1.,0.));
#18708=DIRECTION('ref_axis',(1.,0.,0.));
#18709=DIRECTION('center_axis',(0.,1.,0.));
#18710=DIRECTION('ref_axis',(1.,0.,0.));
#18711=DIRECTION('',(0.,-1.,0.));
#18712=DIRECTION('center_axis',(0.,1.,0.));
#18713=DIRECTION('ref_axis',(1.,0.,0.));
#18714=DIRECTION('center_axis',(0.,1.,0.));
#18715=DIRECTION('ref_axis',(1.,0.,0.));
#18716=DIRECTION('center_axis',(0.,1.,0.));
#18717=DIRECTION('ref_axis',(1.,0.,0.));
#18718=DIRECTION('axis',(0.,0.,1.));
#18719=DIRECTION('refdir',(1.,0.,0.));
#18720=DIRECTION('center_axis',(0.,1.,0.));
#18721=DIRECTION('ref_axis',(1.,0.,0.));
#18722=DIRECTION('center_axis',(0.,-1.,0.));
#18723=DIRECTION('ref_axis',(1.,0.,0.));
#18724=DIRECTION('',(0.,-1.,0.));
#18725=DIRECTION('center_axis',(0.,-1.,0.));
#18726=DIRECTION('ref_axis',(1.,0.,0.));
#18727=DIRECTION('center_axis',(0.,1.,0.));
#18728=DIRECTION('ref_axis',(1.,0.,0.));
#18729=DIRECTION('center_axis',(0.,1.,0.));
#18730=DIRECTION('ref_axis',(1.,0.,0.));
#18731=DIRECTION('',(0.,-1.,0.));
#18732=DIRECTION('center_axis',(0.,1.,0.));
#18733=DIRECTION('ref_axis',(1.,0.,0.));
#18734=DIRECTION('center_axis',(0.,1.,0.));
#18735=DIRECTION('ref_axis',(1.,0.,0.));
#18736=DIRECTION('center_axis',(0.,1.,0.));
#18737=DIRECTION('ref_axis',(1.,0.,0.));
#18738=DIRECTION('axis',(0.,0.,1.));
#18739=DIRECTION('refdir',(1.,0.,0.));
#18740=DIRECTION('center_axis',(0.,1.,0.));
#18741=DIRECTION('ref_axis',(1.,0.,0.));
#18742=DIRECTION('center_axis',(0.,-1.,0.));
#18743=DIRECTION('ref_axis',(1.,0.,0.));
#18744=DIRECTION('',(0.,-1.,0.));
#18745=DIRECTION('center_axis',(0.,-1.,0.));
#18746=DIRECTION('ref_axis',(1.,0.,0.));
#18747=DIRECTION('center_axis',(0.,1.,0.));
#18748=DIRECTION('ref_axis',(1.,0.,0.));
#18749=DIRECTION('center_axis',(0.,1.,0.));
#18750=DIRECTION('ref_axis',(1.,0.,0.));
#18751=DIRECTION('',(0.,-1.,0.));
#18752=DIRECTION('center_axis',(0.,1.,0.));
#18753=DIRECTION('ref_axis',(1.,0.,0.));
#18754=DIRECTION('center_axis',(0.,1.,0.));
#18755=DIRECTION('ref_axis',(1.,0.,0.));
#18756=DIRECTION('center_axis',(0.,1.,0.));
#18757=DIRECTION('ref_axis',(1.,0.,0.));
#18758=DIRECTION('axis',(0.,0.,1.));
#18759=DIRECTION('refdir',(1.,0.,0.));
#18760=DIRECTION('center_axis',(0.,1.,0.));
#18761=DIRECTION('ref_axis',(1.,0.,0.));
#18762=DIRECTION('center_axis',(0.,-1.,0.));
#18763=DIRECTION('ref_axis',(1.,0.,0.));
#18764=DIRECTION('',(0.,-1.,0.));
#18765=DIRECTION('center_axis',(0.,-1.,0.));
#18766=DIRECTION('ref_axis',(1.,0.,0.));
#18767=DIRECTION('center_axis',(0.,1.,0.));
#18768=DIRECTION('ref_axis',(1.,0.,0.));
#18769=DIRECTION('center_axis',(0.,1.,0.));
#18770=DIRECTION('ref_axis',(1.,0.,0.));
#18771=DIRECTION('',(0.,-1.,0.));
#18772=DIRECTION('center_axis',(0.,1.,0.));
#18773=DIRECTION('ref_axis',(1.,0.,0.));
#18774=DIRECTION('center_axis',(0.,1.,0.));
#18775=DIRECTION('ref_axis',(1.,0.,0.));
#18776=DIRECTION('center_axis',(0.,1.,0.));
#18777=DIRECTION('ref_axis',(1.,0.,0.));
#18778=DIRECTION('axis',(0.,0.,1.));
#18779=DIRECTION('refdir',(1.,0.,0.));
#18780=DIRECTION('center_axis',(0.,1.,0.));
#18781=DIRECTION('ref_axis',(1.,0.,0.));
#18782=DIRECTION('center_axis',(0.,1.,0.));
#18783=DIRECTION('ref_axis',(1.,0.,0.));
#18784=DIRECTION('',(0.,1.,0.));
#18785=DIRECTION('center_axis',(0.,1.,0.));
#18786=DIRECTION('ref_axis',(1.,0.,0.));
#18787=DIRECTION('center_axis',(0.,1.,0.));
#18788=DIRECTION('ref_axis',(1.,0.,0.));
#18789=DIRECTION('center_axis',(0.,1.,0.));
#18790=DIRECTION('ref_axis',(1.,0.,0.));
#18791=DIRECTION('center_axis',(0.,1.,0.));
#18792=DIRECTION('ref_axis',(1.,0.,0.));
#18793=DIRECTION('',(0.,1.,0.));
#18794=DIRECTION('center_axis',(0.,-1.,0.));
#18795=DIRECTION('ref_axis',(1.,0.,0.));
#18796=DIRECTION('center_axis',(0.,1.,0.));
#18797=DIRECTION('ref_axis',(1.,0.,0.));
#18798=DIRECTION('center_axis',(0.,1.,0.));
#18799=DIRECTION('ref_axis',(1.,0.,0.));
#18800=DIRECTION('',(0.,1.,0.));
#18801=DIRECTION('center_axis',(0.,-1.,0.));
#18802=DIRECTION('ref_axis',(1.,0.,0.));
#18803=DIRECTION('center_axis',(0.,1.,0.));
#18804=DIRECTION('ref_axis',(1.,0.,0.));
#18805=DIRECTION('center_axis',(0.,1.,0.));
#18806=DIRECTION('ref_axis',(1.,0.,0.));
#18807=DIRECTION('',(0.,1.,0.));
#18808=DIRECTION('center_axis',(0.,-1.,0.));
#18809=DIRECTION('ref_axis',(1.,0.,0.));
#18810=DIRECTION('center_axis',(0.,1.,0.));
#18811=DIRECTION('ref_axis',(1.,0.,0.));
#18812=DIRECTION('center_axis',(0.,1.,0.));
#18813=DIRECTION('ref_axis',(1.,0.,0.));
#18814=DIRECTION('center_axis',(0.,1.,0.));
#18815=DIRECTION('ref_axis',(1.,0.,0.));
#18816=DIRECTION('center_axis',(0.,1.,0.));
#18817=DIRECTION('ref_axis',(1.,0.,0.));
#18818=DIRECTION('center_axis',(0.,1.,0.));
#18819=DIRECTION('ref_axis',(1.,0.,0.));
#18820=DIRECTION('center_axis',(0.,-1.,0.));
#18821=DIRECTION('ref_axis',(1.,0.,0.));
#18822=DIRECTION('center_axis',(0.,1.,0.));
#18823=DIRECTION('ref_axis',(1.,0.,0.));
#18824=DIRECTION('',(0.,-1.,0.));
#18825=DIRECTION('center_axis',(0.,1.,0.));
#18826=DIRECTION('ref_axis',(1.,0.,0.));
#18827=DIRECTION('',(0.,-1.,0.));
#18828=DIRECTION('center_axis',(0.,1.,0.));
#18829=DIRECTION('ref_axis',(1.,0.,0.));
#18830=DIRECTION('center_axis',(0.,1.,0.));
#18831=DIRECTION('ref_axis',(1.,0.,0.));
#18832=DIRECTION('center_axis',(0.,1.,0.));
#18833=DIRECTION('ref_axis',(1.,0.,0.));
#18834=DIRECTION('',(0.,-1.,0.));
#18835=DIRECTION('center_axis',(0.,1.,0.));
#18836=DIRECTION('ref_axis',(1.,0.,0.));
#18837=DIRECTION('center_axis',(0.,1.,0.));
#18838=DIRECTION('ref_axis',(1.,0.,0.));
#18839=DIRECTION('axis',(0.,0.,1.));
#18840=DIRECTION('refdir',(1.,0.,0.));
#18841=DIRECTION('center_axis',(0.,1.,0.));
#18842=DIRECTION('ref_axis',(1.,0.,0.));
#18843=DIRECTION('center_axis',(0.,-1.,0.));
#18844=DIRECTION('ref_axis',(1.,0.,0.));
#18845=DIRECTION('',(0.,-1.,0.));
#18846=DIRECTION('center_axis',(0.,-1.,0.));
#18847=DIRECTION('ref_axis',(1.,0.,0.));
#18848=DIRECTION('center_axis',(0.,1.,0.));
#18849=DIRECTION('ref_axis',(1.,0.,0.));
#18850=DIRECTION('center_axis',(0.,1.,0.));
#18851=DIRECTION('ref_axis',(1.,0.,0.));
#18852=DIRECTION('',(0.,-1.,0.));
#18853=DIRECTION('center_axis',(0.,1.,0.));
#18854=DIRECTION('ref_axis',(1.,0.,0.));
#18855=DIRECTION('center_axis',(0.,1.,0.));
#18856=DIRECTION('ref_axis',(1.,0.,0.));
#18857=DIRECTION('center_axis',(0.,1.,0.));
#18858=DIRECTION('ref_axis',(1.,0.,0.));
#18859=DIRECTION('axis',(0.,0.,1.));
#18860=DIRECTION('refdir',(1.,0.,0.));
#18861=DIRECTION('center_axis',(0.,1.,0.));
#18862=DIRECTION('ref_axis',(1.,0.,0.));
#18863=DIRECTION('center_axis',(0.,-1.,0.));
#18864=DIRECTION('ref_axis',(1.,0.,0.));
#18865=DIRECTION('',(0.,-1.,0.));
#18866=DIRECTION('center_axis',(0.,-1.,0.));
#18867=DIRECTION('ref_axis',(1.,0.,0.));
#18868=DIRECTION('center_axis',(0.,1.,0.));
#18869=DIRECTION('ref_axis',(1.,0.,0.));
#18870=DIRECTION('center_axis',(0.,1.,0.));
#18871=DIRECTION('ref_axis',(1.,0.,0.));
#18872=DIRECTION('',(0.,-1.,0.));
#18873=DIRECTION('center_axis',(0.,1.,0.));
#18874=DIRECTION('ref_axis',(1.,0.,0.));
#18875=DIRECTION('center_axis',(0.,1.,0.));
#18876=DIRECTION('ref_axis',(1.,0.,0.));
#18877=DIRECTION('center_axis',(0.,1.,0.));
#18878=DIRECTION('ref_axis',(1.,0.,0.));
#18879=DIRECTION('axis',(0.,0.,1.));
#18880=DIRECTION('refdir',(1.,0.,0.));
#18881=DIRECTION('center_axis',(0.,1.,0.));
#18882=DIRECTION('ref_axis',(1.,0.,0.));
#18883=DIRECTION('center_axis',(0.,-1.,0.));
#18884=DIRECTION('ref_axis',(1.,0.,0.));
#18885=DIRECTION('',(0.,-1.,0.));
#18886=DIRECTION('center_axis',(0.,-1.,0.));
#18887=DIRECTION('ref_axis',(1.,0.,0.));
#18888=DIRECTION('center_axis',(0.,1.,0.));
#18889=DIRECTION('ref_axis',(1.,0.,0.));
#18890=DIRECTION('center_axis',(0.,1.,0.));
#18891=DIRECTION('ref_axis',(1.,0.,0.));
#18892=DIRECTION('',(0.,-1.,0.));
#18893=DIRECTION('center_axis',(0.,1.,0.));
#18894=DIRECTION('ref_axis',(1.,0.,0.));
#18895=DIRECTION('center_axis',(0.,1.,0.));
#18896=DIRECTION('ref_axis',(1.,0.,0.));
#18897=DIRECTION('center_axis',(0.,1.,0.));
#18898=DIRECTION('ref_axis',(1.,0.,0.));
#18899=DIRECTION('axis',(0.,0.,1.));
#18900=DIRECTION('refdir',(1.,0.,0.));
#18901=DIRECTION('center_axis',(0.,1.,0.));
#18902=DIRECTION('ref_axis',(0.,0.,1.));
#18903=DIRECTION('center_axis',(0.,-1.,0.));
#18904=DIRECTION('ref_axis',(1.,0.,0.));
#18905=DIRECTION('center_axis',(0.,-1.,0.));
#18906=DIRECTION('ref_axis',(1.,0.,0.));
#18907=DIRECTION('center_axis',(0.,-1.,0.));
#18908=DIRECTION('ref_axis',(1.,0.,0.));
#18909=DIRECTION('',(0.707106781186547,0.707106781186548,8.65956056235493E-17));
#18910=DIRECTION('center_axis',(0.,-1.,0.));
#18911=DIRECTION('ref_axis',(1.,0.,0.));
#18912=DIRECTION('center_axis',(0.,-1.,0.));
#18913=DIRECTION('ref_axis',(1.,0.,0.));
#18914=DIRECTION('',(0.,1.,0.));
#18915=DIRECTION('center_axis',(0.,1.,0.));
#18916=DIRECTION('ref_axis',(1.,0.,0.));
#18917=DIRECTION('center_axis',(0.,-1.,0.));
#18918=DIRECTION('ref_axis',(1.,0.,0.));
#18919=DIRECTION('',(-0.707106781186547,0.707106781186548,-8.65956056235493E-17));
#18920=DIRECTION('center_axis',(0.,-1.,0.));
#18921=DIRECTION('ref_axis',(0.,0.,-1.));
#18922=DIRECTION('center_axis',(0.,-1.,0.));
#18923=DIRECTION('ref_axis',(1.,0.,0.));
#18924=DIRECTION('center_axis',(0.,1.,0.));
#18925=DIRECTION('ref_axis',(1.,0.,0.));
#18926=DIRECTION('center_axis',(0.,1.,0.));
#18927=DIRECTION('ref_axis',(1.,0.,0.));
#18928=DIRECTION('',(-0.447213595499958,0.894427190999916,-5.47678698264203E-17));
#18929=DIRECTION('center_axis',(0.,-1.,0.));
#18930=DIRECTION('ref_axis',(1.,0.,0.));
#18931=DIRECTION('center_axis',(0.,1.,0.));
#18932=DIRECTION('ref_axis',(1.,0.,0.));
#18933=DIRECTION('',(0.,1.,0.));
#18934=DIRECTION('center_axis',(0.,1.,0.));
#18935=DIRECTION('ref_axis',(1.,0.,0.));
#18936=DIRECTION('center_axis',(0.,-1.,0.));
#18937=DIRECTION('ref_axis',(1.,0.,0.));
#18938=DIRECTION('',(-0.707106781186547,0.707106781186548,-8.65956056235493E-17));
#18939=DIRECTION('center_axis',(0.,-1.,0.));
#18940=DIRECTION('ref_axis',(0.,0.,-1.));
#18941=DIRECTION('center_axis',(0.866025403784439,0.,-0.5));
#18942=DIRECTION('ref_axis',(0.5,0.,0.866025403784439));
#18943=DIRECTION('',(-0.5,0.,-0.866025403784439));
#18944=DIRECTION('',(0.,-1.,0.));
#18945=DIRECTION('',(0.5,0.,0.866025403784439));
#18946=DIRECTION('',(0.,-1.,0.));
#18947=DIRECTION('center_axis',(1.60246890531964E-16,0.,-1.));
#18948=DIRECTION('ref_axis',(1.,0.,1.60246890531964E-16));
#18949=DIRECTION('',(-1.,0.,-1.60246890531964E-16));
#18950=DIRECTION('',(0.,-1.,0.));
#18951=DIRECTION('',(1.,0.,1.60246890531964E-16));
#18952=DIRECTION('center_axis',(-0.866025403784439,0.,-0.5));
#18953=DIRECTION('ref_axis',(0.5,0.,-0.866025403784439));
#18954=DIRECTION('',(-0.5,0.,0.866025403784439));
#18955=DIRECTION('',(0.,-1.,0.));
#18956=DIRECTION('',(0.5,0.,-0.866025403784439));
#18957=DIRECTION('center_axis',(-0.866025403784439,0.,0.5));
#18958=DIRECTION('ref_axis',(-0.5,0.,-0.866025403784439));
#18959=DIRECTION('',(0.5,0.,0.866025403784439));
#18960=DIRECTION('',(0.,-1.,0.));
#18961=DIRECTION('',(-0.5,0.,-0.866025403784439));
#18962=DIRECTION('center_axis',(-1.60246890531964E-16,0.,1.));
#18963=DIRECTION('ref_axis',(-1.,0.,-1.60246890531964E-16));
#18964=DIRECTION('',(1.,0.,1.60246890531964E-16));
#18965=DIRECTION('',(0.,-1.,0.));
#18966=DIRECTION('',(-1.,0.,-1.60246890531964E-16));
#18967=DIRECTION('center_axis',(0.866025403784439,0.,0.5));
#18968=DIRECTION('ref_axis',(-0.5,0.,0.866025403784439));
#18969=DIRECTION('',(0.5,0.,-0.866025403784439));
#18970=DIRECTION('',(-0.5,0.,0.866025403784439));
#18971=DIRECTION('center_axis',(0.,1.,0.));
#18972=DIRECTION('ref_axis',(1.,0.,0.));
#18973=DIRECTION('center_axis',(0.,-1.,0.));
#18974=DIRECTION('ref_axis',(0.,0.,-1.));
#18975=DIRECTION('',(0.,0.,1.));
#18976=DIRECTION('',(1.,0.,0.));
#18977=DIRECTION('',(0.,0.,1.));
#18978=DIRECTION('',(1.,0.,0.));
#18979=DIRECTION('',(0.,0.,1.));
#18980=DIRECTION('',(1.,0.,0.));
#18981=DIRECTION('',(0.,0.,1.));
#18982=DIRECTION('',(1.,0.,0.));
#18983=DIRECTION('',(0.,0.,1.));
#18984=DIRECTION('',(1.,0.,0.));
#18985=DIRECTION('',(0.,0.,1.));
#18986=DIRECTION('',(1.,0.,0.));
#18987=DIRECTION('',(0.,0.,1.));
#18988=DIRECTION('',(1.,0.,0.));
#18989=DIRECTION('',(0.,0.,1.));
#18990=DIRECTION('',(1.,0.,0.));
#18991=DIRECTION('',(0.,0.,1.));
#18992=DIRECTION('',(1.,0.,0.));
#18993=DIRECTION('',(0.,0.,1.));
#18994=DIRECTION('',(1.,0.,0.));
#18995=DIRECTION('',(0.,0.,1.));
#18996=DIRECTION('',(1.,0.,0.));
#18997=DIRECTION('',(0.,0.,1.));
#18998=DIRECTION('',(1.,0.,0.));
#18999=DIRECTION('',(0.,0.,1.));
#19000=DIRECTION('',(1.,0.,0.));
#19001=DIRECTION('',(0.,0.,1.));
#19002=DIRECTION('',(1.,0.,0.));
#19003=DIRECTION('',(0.,0.,1.));
#19004=DIRECTION('',(1.,0.,0.));
#19005=DIRECTION('',(0.,0.,1.));
#19006=DIRECTION('',(1.,0.,0.));
#19007=DIRECTION('',(0.,0.,1.));
#19008=DIRECTION('',(1.,0.,0.));
#19009=DIRECTION('',(0.,0.,1.));
#19010=DIRECTION('',(1.,0.,0.));
#19011=DIRECTION('',(0.,0.,1.));
#19012=DIRECTION('',(1.,0.,0.));
#19013=DIRECTION('',(0.,0.,1.));
#19014=DIRECTION('',(1.,0.,0.));
#19015=DIRECTION('',(0.,0.,1.));
#19016=DIRECTION('',(1.,0.,0.));
#19017=DIRECTION('',(0.,0.,1.));
#19018=DIRECTION('',(1.,0.,0.));
#19019=DIRECTION('',(0.,0.,1.));
#19020=DIRECTION('',(1.,0.,0.));
#19021=DIRECTION('',(0.,0.,1.));
#19022=DIRECTION('',(1.,0.,0.));
#19023=DIRECTION('',(0.,0.,1.));
#19024=DIRECTION('',(1.,0.,0.));
#19025=DIRECTION('',(0.,0.,1.));
#19026=DIRECTION('',(1.,0.,0.));
#19027=DIRECTION('',(0.,0.,1.));
#19028=DIRECTION('',(1.,0.,0.));
#19029=DIRECTION('',(0.,0.,1.));
#19030=DIRECTION('',(1.,0.,0.));
#19031=DIRECTION('',(0.,0.,1.));
#19032=DIRECTION('',(1.,0.,0.));
#19033=DIRECTION('',(0.,-1.,2.22044604925031E-16));
#19034=DIRECTION('',(1.,0.,0.));
#19035=DIRECTION('',(0.,-1.,2.22044604925031E-16));
#19036=DIRECTION('',(1.,0.,0.));
#19037=DIRECTION('',(0.,-1.,2.22044604925031E-16));
#19038=DIRECTION('',(1.,0.,0.));
#19039=DIRECTION('',(0.,-1.,2.22044604925031E-16));
#19040=DIRECTION('',(1.,0.,0.));
#19041=DIRECTION('',(0.,-1.,2.22044604925031E-16));
#19042=DIRECTION('',(1.,0.,0.));
#19043=DIRECTION('',(0.,-1.,2.22044604925031E-16));
#19044=DIRECTION('',(1.,0.,0.));
#19045=DIRECTION('',(0.,-1.,2.22044604925031E-16));
#19046=DIRECTION('',(1.,0.,0.));
#19047=DIRECTION('',(0.,-1.,2.22044604925031E-16));
#19048=DIRECTION('',(1.,0.,0.));
#19049=DIRECTION('',(0.,0.,1.));
#19050=DIRECTION('',(-1.,1.22464679914735E-16,0.));
#19051=DIRECTION('',(0.,0.,1.));
#19052=DIRECTION('',(-1.,1.22464679914735E-16,0.));
#19053=DIRECTION('',(0.,0.,1.));
#19054=DIRECTION('',(-1.,1.22464679914735E-16,0.));
#19055=DIRECTION('',(0.,0.,1.));
#19056=DIRECTION('',(-1.,1.22464679914735E-16,0.));
#19057=DIRECTION('',(0.,0.,1.));
#19058=DIRECTION('',(-1.,1.22464679914735E-16,0.));
#19059=DIRECTION('',(0.,0.,1.));
#19060=DIRECTION('',(-1.,1.22464679914735E-16,0.));
#19061=DIRECTION('',(0.,0.,1.));
#19062=DIRECTION('',(-1.,1.22464679914735E-16,0.));
#19063=DIRECTION('',(0.,0.,1.));
#19064=DIRECTION('',(-1.,1.22464679914735E-16,0.));
#19065=DIRECTION('',(0.,0.,1.));
#19066=DIRECTION('',(2.22044604925031E-16,-1.,0.));
#19067=DIRECTION('',(0.,-1.,2.22044604925031E-16));
#19068=DIRECTION('',(1.,0.,0.));
#19069=DIRECTION('',(0.,-1.,2.22044604925031E-16));
#19070=DIRECTION('',(1.,0.,0.));
#19071=DIRECTION('',(0.,0.,1.));
#19072=DIRECTION('',(2.22044604925031E-16,-1.,0.));
#19073=DIRECTION('',(0.,-1.,2.22044604925031E-16));
#19074=DIRECTION('',(1.,0.,0.));
#19075=DIRECTION('',(0.,-1.,2.22044604925031E-16));
#19076=DIRECTION('',(1.,0.,0.));
#19077=DIRECTION('',(0.,0.,1.));
#19078=DIRECTION('',(1.,0.,0.));
#19079=DIRECTION('',(0.,0.,1.));
#19080=DIRECTION('',(1.,0.,0.));
#19081=DIRECTION('',(0.,0.,1.));
#19082=DIRECTION('',(1.,0.,0.));
#19083=DIRECTION('',(0.,0.,1.));
#19084=DIRECTION('',(1.,0.,0.));
#19085=DIRECTION('',(0.,0.,1.));
#19086=DIRECTION('',(1.,0.,0.));
#19087=DIRECTION('',(0.,0.,1.));
#19088=DIRECTION('',(1.,0.,0.));
#19089=DIRECTION('',(0.,0.,1.));
#19090=DIRECTION('',(1.,0.,0.));
#19091=DIRECTION('',(0.,0.,1.));
#19092=DIRECTION('',(1.,0.,0.));
#19093=DIRECTION('',(0.,0.,1.));
#19094=DIRECTION('',(1.,0.,0.));
#19095=DIRECTION('',(0.,0.,1.));
#19096=DIRECTION('',(1.,0.,0.));
#19097=DIRECTION('',(0.,0.,1.));
#19098=DIRECTION('',(1.,0.,0.));
#19099=DIRECTION('',(0.,0.,1.));
#19100=DIRECTION('',(1.,0.,0.));
#19101=DIRECTION('',(0.,0.,1.));
#19102=DIRECTION('',(-1.,1.22464679914735E-16,0.));
#19103=DIRECTION('',(0.,0.,1.));
#19104=DIRECTION('',(-1.,1.22464679914735E-16,0.));
#19105=DIRECTION('',(0.,0.,1.));
#19106=DIRECTION('',(-1.,1.22464679914735E-16,0.));
#19107=DIRECTION('',(0.,0.,1.));
#19108=DIRECTION('',(-1.,1.22464679914735E-16,0.));
#19109=DIRECTION('',(0.,0.,1.));
#19110=DIRECTION('',(-1.,1.22464679914735E-16,0.));
#19111=DIRECTION('',(0.,0.,1.));
#19112=DIRECTION('',(-1.,1.22464679914735E-16,0.));
#19113=DIRECTION('',(0.,0.,1.));
#19114=DIRECTION('',(-1.,1.22464679914735E-16,0.));
#19115=DIRECTION('',(0.,0.,1.));
#19116=DIRECTION('',(-1.,1.22464679914735E-16,0.));
#19117=DIRECTION('axis',(0.,0.,1.));
#19118=DIRECTION('refdir',(1.,0.,0.));
#19119=DIRECTION('axis',(0.,0.,1.));
#19120=DIRECTION('refdir',(1.,0.,0.));
#19121=DIRECTION('center_axis',(1.,0.,0.));
#19122=DIRECTION('ref_axis',(0.,0.,-1.));
#19123=DIRECTION('center_axis',(1.,0.,0.));
#19124=DIRECTION('ref_axis',(0.,0.,-1.));
#19125=DIRECTION('',(1.,0.,0.));
#19126=DIRECTION('center_axis',(-1.,0.,0.));
#19127=DIRECTION('ref_axis',(0.,0.,-1.));
#19128=DIRECTION('center_axis',(1.,0.,0.));
#19129=DIRECTION('ref_axis',(0.,0.,-1.));
#19130=DIRECTION('center_axis',(1.,0.,0.));
#19131=DIRECTION('ref_axis',(0.,0.,-1.));
#19132=DIRECTION('',(1.,0.,0.));
#19133=DIRECTION('center_axis',(-1.,0.,0.));
#19134=DIRECTION('ref_axis',(0.,0.,-1.));
#19135=DIRECTION('center_axis',(1.,0.,0.));
#19136=DIRECTION('ref_axis',(0.,0.,-1.));
#19137=DIRECTION('center_axis',(1.,0.,0.));
#19138=DIRECTION('ref_axis',(0.,0.,-1.));
#19139=DIRECTION('',(1.,0.,0.));
#19140=DIRECTION('center_axis',(-1.,0.,0.));
#19141=DIRECTION('ref_axis',(0.,0.,-1.));
#19142=DIRECTION('center_axis',(0.,1.,0.));
#19143=DIRECTION('ref_axis',(-1.,0.,0.));
#19144=DIRECTION('',(-1.,0.,0.));
#19145=DIRECTION('',(0.,0.,1.));
#19146=DIRECTION('',(-1.,0.,0.));
#19147=DIRECTION('',(0.,0.,1.));
#19148=DIRECTION('center_axis',(1.,0.,0.));
#19149=DIRECTION('ref_axis',(0.,1.,0.));
#19150=DIRECTION('',(0.,1.,0.));
#19151=DIRECTION('',(0.,1.,0.));
#19152=DIRECTION('',(0.,0.,1.));
#19153=DIRECTION('center_axis',(0.,-1.,0.));
#19154=DIRECTION('ref_axis',(1.,0.,0.));
#19155=DIRECTION('',(1.,0.,0.));
#19156=DIRECTION('',(1.,0.,0.));
#19157=DIRECTION('',(0.,0.,1.));
#19158=DIRECTION('center_axis',(-1.,0.,0.));
#19159=DIRECTION('ref_axis',(0.,-1.,0.));
#19160=DIRECTION('',(0.,-1.,0.));
#19161=DIRECTION('',(0.,-1.,0.));
#19162=DIRECTION('center_axis',(0.,0.,1.));
#19163=DIRECTION('ref_axis',(1.,0.,0.));
#19164=DIRECTION('center_axis',(0.,0.,1.));
#19165=DIRECTION('ref_axis',(1.,0.,0.));
#19166=DIRECTION('axis',(0.,0.,1.));
#19167=DIRECTION('refdir',(1.,0.,0.));
#19168=DIRECTION('center_axis',(1.,0.,0.));
#19169=DIRECTION('ref_axis',(0.,0.,-1.));
#19170=DIRECTION('center_axis',(1.,0.,0.));
#19171=DIRECTION('ref_axis',(0.,0.,-1.));
#19172=DIRECTION('',(1.,0.,0.));
#19173=DIRECTION('center_axis',(-1.,0.,0.));
#19174=DIRECTION('ref_axis',(0.,0.,-1.));
#19175=DIRECTION('center_axis',(1.,0.,0.));
#19176=DIRECTION('ref_axis',(0.,0.,-1.));
#19177=DIRECTION('center_axis',(1.,0.,0.));
#19178=DIRECTION('ref_axis',(0.,0.,-1.));
#19179=DIRECTION('',(1.,0.,0.));
#19180=DIRECTION('center_axis',(-1.,0.,0.));
#19181=DIRECTION('ref_axis',(0.,0.,-1.));
#19182=DIRECTION('center_axis',(1.,0.,0.));
#19183=DIRECTION('ref_axis',(0.,0.,-1.));
#19184=DIRECTION('center_axis',(1.,0.,0.));
#19185=DIRECTION('ref_axis',(0.,0.,-1.));
#19186=DIRECTION('',(1.,0.,0.));
#19187=DIRECTION('center_axis',(-1.,0.,0.));
#19188=DIRECTION('ref_axis',(0.,0.,-1.));
#19189=DIRECTION('center_axis',(0.,0.,1.));
#19190=DIRECTION('ref_axis',(0.,-1.,0.));
#19191=DIRECTION('',(0.,-1.,0.));
#19192=DIRECTION('',(1.,0.,0.));
#19193=DIRECTION('',(0.,-1.,0.));
#19194=DIRECTION('',(1.,0.,0.));
#19195=DIRECTION('center_axis',(0.,1.,0.));
#19196=DIRECTION('ref_axis',(0.,0.,1.));
#19197=DIRECTION('',(0.,0.,1.));
#19198=DIRECTION('',(0.,0.,1.));
#19199=DIRECTION('',(1.,0.,0.));
#19200=DIRECTION('center_axis',(0.,0.,-1.));
#19201=DIRECTION('ref_axis',(0.,1.,0.));
#19202=DIRECTION('',(0.,1.,0.));
#19203=DIRECTION('',(0.,1.,0.));
#19204=DIRECTION('',(1.,0.,0.));
#19205=DIRECTION('center_axis',(0.,-1.,0.));
#19206=DIRECTION('ref_axis',(0.,0.,-1.));
#19207=DIRECTION('',(0.,0.,-1.));
#19208=DIRECTION('',(0.,0.,-1.));
#19209=DIRECTION('center_axis',(1.,0.,0.));
#19210=DIRECTION('ref_axis',(0.,0.,-1.));
#19211=DIRECTION('center_axis',(1.,0.,0.));
#19212=DIRECTION('ref_axis',(0.,0.,-1.));
#19213=DIRECTION('axis',(0.,0.,1.));
#19214=DIRECTION('refdir',(1.,0.,0.));
#19215=DIRECTION('center_axis',(1.,0.,0.));
#19216=DIRECTION('ref_axis',(0.,0.,-1.));
#19217=DIRECTION('center_axis',(1.,0.,0.));
#19218=DIRECTION('ref_axis',(0.,0.,-1.));
#19219=DIRECTION('',(1.,0.,0.));
#19220=DIRECTION('center_axis',(-1.,0.,0.));
#19221=DIRECTION('ref_axis',(0.,0.,-1.));
#19222=DIRECTION('center_axis',(1.,0.,0.));
#19223=DIRECTION('ref_axis',(0.,0.,-1.));
#19224=DIRECTION('center_axis',(1.,0.,0.));
#19225=DIRECTION('ref_axis',(0.,0.,-1.));
#19226=DIRECTION('',(1.,0.,0.));
#19227=DIRECTION('center_axis',(-1.,0.,0.));
#19228=DIRECTION('ref_axis',(0.,0.,-1.));
#19229=DIRECTION('center_axis',(1.,0.,0.));
#19230=DIRECTION('ref_axis',(0.,0.,-1.));
#19231=DIRECTION('center_axis',(1.,0.,0.));
#19232=DIRECTION('ref_axis',(0.,0.,-1.));
#19233=DIRECTION('',(1.,0.,0.));
#19234=DIRECTION('center_axis',(-1.,0.,0.));
#19235=DIRECTION('ref_axis',(0.,0.,-1.));
#19236=DIRECTION('center_axis',(0.,0.,1.));
#19237=DIRECTION('ref_axis',(0.,-1.,0.));
#19238=DIRECTION('',(0.,-1.,0.));
#19239=DIRECTION('',(1.,0.,0.));
#19240=DIRECTION('',(0.,-1.,0.));
#19241=DIRECTION('',(1.,0.,0.));
#19242=DIRECTION('center_axis',(0.,1.,0.));
#19243=DIRECTION('ref_axis',(0.,0.,1.));
#19244=DIRECTION('',(0.,0.,1.));
#19245=DIRECTION('',(0.,0.,1.));
#19246=DIRECTION('',(1.,0.,0.));
#19247=DIRECTION('center_axis',(0.,0.,-1.));
#19248=DIRECTION('ref_axis',(0.,1.,0.));
#19249=DIRECTION('',(0.,1.,0.));
#19250=DIRECTION('',(0.,1.,0.));
#19251=DIRECTION('',(1.,0.,0.));
#19252=DIRECTION('center_axis',(0.,-1.,0.));
#19253=DIRECTION('ref_axis',(0.,0.,-1.));
#19254=DIRECTION('',(0.,0.,-1.));
#19255=DIRECTION('',(0.,0.,-1.));
#19256=DIRECTION('center_axis',(1.,0.,0.));
#19257=DIRECTION('ref_axis',(0.,0.,-1.));
#19258=DIRECTION('center_axis',(1.,0.,0.));
#19259=DIRECTION('ref_axis',(0.,0.,-1.));
#19260=DIRECTION('axis',(0.,0.,1.));
#19261=DIRECTION('refdir',(1.,0.,0.));
#19262=DIRECTION('center_axis',(0.,1.,0.));
#19263=DIRECTION('ref_axis',(1.,0.,0.));
#19264=DIRECTION('center_axis',(0.,1.,0.));
#19265=DIRECTION('ref_axis',(1.,0.,0.));
#19266=DIRECTION('',(0.,1.,0.));
#19267=DIRECTION('center_axis',(0.,-1.,0.));
#19268=DIRECTION('ref_axis',(1.,0.,0.));
#19269=DIRECTION('center_axis',(0.,1.,0.));
#19270=DIRECTION('ref_axis',(-1.,0.,0.));
#19271=DIRECTION('',(-1.,0.,0.));
#19272=DIRECTION('',(0.,0.,1.));
#19273=DIRECTION('',(-1.,0.,0.));
#19274=DIRECTION('',(0.,0.,1.));
#19275=DIRECTION('center_axis',(1.,0.,0.));
#19276=DIRECTION('ref_axis',(0.,1.,0.));
#19277=DIRECTION('',(0.,1.,0.));
#19278=DIRECTION('',(0.,1.,0.));
#19279=DIRECTION('',(0.,0.,1.));
#19280=DIRECTION('center_axis',(0.,-1.,0.));
#19281=DIRECTION('ref_axis',(1.,0.,0.));
#19282=DIRECTION('',(1.,0.,0.));
#19283=DIRECTION('',(1.,0.,0.));
#19284=DIRECTION('',(0.,0.,1.));
#19285=DIRECTION('center_axis',(-1.,0.,0.));
#19286=DIRECTION('ref_axis',(0.,-1.,0.));
#19287=DIRECTION('',(0.,-1.,0.));
#19288=DIRECTION('',(0.,-1.,0.));
#19289=DIRECTION('center_axis',(0.,0.,1.));
#19290=DIRECTION('ref_axis',(1.,0.,0.));
#19291=DIRECTION('center_axis',(0.,0.,1.));
#19292=DIRECTION('ref_axis',(1.,0.,0.));
#19293=DIRECTION('axis',(0.,0.,1.));
#19294=DIRECTION('refdir',(1.,0.,0.));
#19295=DIRECTION('center_axis',(0.,1.,0.));
#19296=DIRECTION('ref_axis',(1.,0.,0.));
#19297=DIRECTION('center_axis',(0.,1.,0.));
#19298=DIRECTION('ref_axis',(1.,0.,0.));
#19299=DIRECTION('',(0.,1.,0.));
#19300=DIRECTION('center_axis',(0.,-1.,0.));
#19301=DIRECTION('ref_axis',(1.,0.,0.));
#19302=DIRECTION('center_axis',(0.,1.,0.));
#19303=DIRECTION('ref_axis',(1.,0.,0.));
#19304=DIRECTION('center_axis',(0.,1.,0.));
#19305=DIRECTION('ref_axis',(1.,0.,0.));
#19306=DIRECTION('center_axis',(0.,1.,0.));
#19307=DIRECTION('ref_axis',(1.,0.,0.));
#19308=DIRECTION('center_axis',(0.,1.,0.));
#19309=DIRECTION('ref_axis',(1.,0.,0.));
#19310=DIRECTION('center_axis',(0.,1.,0.));
#19311=DIRECTION('ref_axis',(1.,0.,0.));
#19312=DIRECTION('',(0.,-1.,0.));
#19313=DIRECTION('center_axis',(0.,1.,0.));
#19314=DIRECTION('ref_axis',(1.,0.,0.));
#19315=DIRECTION('center_axis',(0.,1.,0.));
#19316=DIRECTION('ref_axis',(1.,0.,0.));
#19317=DIRECTION('center_axis',(0.,1.,0.));
#19318=DIRECTION('ref_axis',(1.,0.,0.));
#19319=DIRECTION('center_axis',(0.,1.,0.));
#19320=DIRECTION('ref_axis',(1.,0.,0.));
#19321=DIRECTION('',(0.,-1.,0.));
#19322=DIRECTION('center_axis',(0.,1.,0.));
#19323=DIRECTION('ref_axis',(1.,0.,0.));
#19324=DIRECTION('axis',(0.,0.,1.));
#19325=DIRECTION('refdir',(1.,0.,0.));
#19326=DIRECTION('center_axis',(0.,1.,0.));
#19327=DIRECTION('ref_axis',(1.,0.,0.));
#19328=DIRECTION('center_axis',(0.,-1.,0.));
#19329=DIRECTION('ref_axis',(1.,0.,0.));
#19330=DIRECTION('',(0.,-1.,0.));
#19331=DIRECTION('center_axis',(0.,-1.,0.));
#19332=DIRECTION('ref_axis',(1.,0.,0.));
#19333=DIRECTION('center_axis',(0.,1.,0.));
#19334=DIRECTION('ref_axis',(1.,0.,0.));
#19335=DIRECTION('center_axis',(0.,1.,0.));
#19336=DIRECTION('ref_axis',(1.,0.,0.));
#19337=DIRECTION('',(0.,-1.,0.));
#19338=DIRECTION('center_axis',(0.,1.,0.));
#19339=DIRECTION('ref_axis',(1.,0.,0.));
#19340=DIRECTION('center_axis',(0.,1.,0.));
#19341=DIRECTION('ref_axis',(1.,0.,0.));
#19342=DIRECTION('center_axis',(0.,1.,0.));
#19343=DIRECTION('ref_axis',(1.,0.,0.));
#19344=DIRECTION('axis',(0.,0.,1.));
#19345=DIRECTION('refdir',(1.,0.,0.));
#19346=DIRECTION('center_axis',(0.,1.,0.));
#19347=DIRECTION('ref_axis',(1.,0.,0.));
#19348=DIRECTION('center_axis',(0.,-1.,0.));
#19349=DIRECTION('ref_axis',(1.,0.,0.));
#19350=DIRECTION('',(0.,-1.,0.));
#19351=DIRECTION('center_axis',(0.,-1.,0.));
#19352=DIRECTION('ref_axis',(1.,0.,0.));
#19353=DIRECTION('center_axis',(0.,1.,0.));
#19354=DIRECTION('ref_axis',(1.,0.,0.));
#19355=DIRECTION('center_axis',(0.,1.,0.));
#19356=DIRECTION('ref_axis',(1.,0.,0.));
#19357=DIRECTION('',(0.,-1.,0.));
#19358=DIRECTION('center_axis',(0.,1.,0.));
#19359=DIRECTION('ref_axis',(1.,0.,0.));
#19360=DIRECTION('center_axis',(0.,1.,0.));
#19361=DIRECTION('ref_axis',(1.,0.,0.));
#19362=DIRECTION('center_axis',(0.,1.,0.));
#19363=DIRECTION('ref_axis',(1.,0.,0.));
#19364=DIRECTION('axis',(0.,0.,1.));
#19365=DIRECTION('refdir',(1.,0.,0.));
#19366=DIRECTION('axis',(0.,0.,1.));
#19367=DIRECTION('refdir',(1.,0.,0.));
#19368=DIRECTION('center_axis',(0.,1.,0.));
#19369=DIRECTION('ref_axis',(0.,0.,1.));
#19370=DIRECTION('center_axis',(0.,-1.,0.));
#19371=DIRECTION('ref_axis',(1.,0.,0.));
#19372=DIRECTION('',(-1.,0.,0.));
#19373=DIRECTION('',(0.,0.,-1.));
#19374=DIRECTION('',(1.,0.,0.));
#19375=DIRECTION('center_axis',(0.,0.,1.));
#19376=DIRECTION('ref_axis',(1.,0.,0.));
#19377=DIRECTION('',(0.,-1.,0.));
#19378=DIRECTION('',(0.,1.,0.));
#19379=DIRECTION('',(-1.,0.,0.));
#19380=DIRECTION('center_axis',(0.,-1.,0.));
#19381=DIRECTION('ref_axis',(0.,0.,-1.));
#19382=DIRECTION('center_axis',(0.,1.,0.));
#19383=DIRECTION('ref_axis',(1.,0.,0.));
#19384=DIRECTION('',(0.,0.,1.));
#19385=DIRECTION('',(1.,0.,0.));
#19386=DIRECTION('center_axis',(0.,0.,-1.));
#19387=DIRECTION('ref_axis',(-1.,0.,0.));
#19388=DIRECTION('',(0.,1.,0.));
#19389=DIRECTION('',(0.,1.,0.));
#19390=DIRECTION('center_axis',(1.,0.,0.));
#19391=DIRECTION('ref_axis',(0.,0.,-1.));
#19392=DIRECTION('center_axis',(0.,1.,0.));
#19393=DIRECTION('ref_axis',(0.,0.,1.));
#19394=DIRECTION('center_axis',(0.,-1.,0.));
#19395=DIRECTION('ref_axis',(1.,0.,0.));
#19396=DIRECTION('center_axis',(0.,-1.,0.));
#19397=DIRECTION('ref_axis',(1.,0.,0.));
#19398=DIRECTION('center_axis',(0.,-1.,0.));
#19399=DIRECTION('ref_axis',(1.,0.,0.));
#19400=DIRECTION('center_axis',(0.,-1.,0.));
#19401=DIRECTION('ref_axis',(1.,0.,0.));
#19402=DIRECTION('',(0.,1.,0.));
#19403=DIRECTION('center_axis',(0.,-1.,0.));
#19404=DIRECTION('ref_axis',(0.,0.,-1.));
#19405=DIRECTION('center_axis',(0.,-1.,0.));
#19406=DIRECTION('ref_axis',(1.,0.,0.));
#19407=DIRECTION('center_axis',(0.,-1.,0.));
#19408=DIRECTION('ref_axis',(1.,0.,0.));
#19409=DIRECTION('center_axis',(0.,-1.,0.));
#19410=DIRECTION('ref_axis',(1.,0.,0.));
#19411=DIRECTION('',(0.,1.,0.));
#19412=DIRECTION('center_axis',(0.,1.,0.));
#19413=DIRECTION('ref_axis',(0.,0.,1.));
#19414=DIRECTION('center_axis',(0.,-1.,0.));
#19415=DIRECTION('ref_axis',(1.,0.,0.));
#19416=DIRECTION('center_axis',(0.,-1.,0.));
#19417=DIRECTION('ref_axis',(1.,0.,0.));
#19418=DIRECTION('center_axis',(0.,-1.,0.));
#19419=DIRECTION('ref_axis',(1.,0.,0.));
#19420=DIRECTION('',(0.,1.,0.));
#19421=DIRECTION('center_axis',(0.,-1.,0.));
#19422=DIRECTION('ref_axis',(0.,0.,-1.));
#19423=DIRECTION('center_axis',(0.,-1.,0.));
#19424=DIRECTION('ref_axis',(1.,0.,0.));
#19425=DIRECTION('center_axis',(0.,-1.,0.));
#19426=DIRECTION('ref_axis',(1.,0.,0.));
#19427=DIRECTION('center_axis',(0.,-1.,0.));
#19428=DIRECTION('ref_axis',(1.,0.,0.));
#19429=DIRECTION('',(0.,1.,0.));
#19430=DIRECTION('center_axis',(0.,1.,0.));
#19431=DIRECTION('ref_axis',(0.,0.,1.));
#19432=DIRECTION('center_axis',(0.,-1.,0.));
#19433=DIRECTION('ref_axis',(1.,0.,0.));
#19434=DIRECTION('center_axis',(0.,-1.,0.));
#19435=DIRECTION('ref_axis',(1.,0.,0.));
#19436=DIRECTION('center_axis',(0.,-1.,0.));
#19437=DIRECTION('ref_axis',(1.,0.,0.));
#19438=DIRECTION('',(0.,1.,0.));
#19439=DIRECTION('center_axis',(0.,-1.,0.));
#19440=DIRECTION('ref_axis',(0.,0.,-1.));
#19441=DIRECTION('center_axis',(0.,-1.,0.));
#19442=DIRECTION('ref_axis',(1.,0.,0.));
#19443=DIRECTION('center_axis',(0.,-1.,0.));
#19444=DIRECTION('ref_axis',(1.,0.,0.));
#19445=DIRECTION('',(0.,1.,0.));
#19446=DIRECTION('axis',(0.,0.,1.));
#19447=DIRECTION('refdir',(1.,0.,0.));
#19448=DIRECTION('center_axis',(0.,1.,0.));
#19449=DIRECTION('ref_axis',(0.,0.,1.));
#19450=DIRECTION('center_axis',(0.,1.,0.));
#19451=DIRECTION('ref_axis',(1.,0.,0.));
#19452=DIRECTION('',(1.,0.,0.));
#19453=DIRECTION('center_axis',(0.,-1.,0.));
#19454=DIRECTION('ref_axis',(1.,0.,0.));
#19455=DIRECTION('',(-1.,0.,0.));
#19456=DIRECTION('center_axis',(0.,0.,-1.));
#19457=DIRECTION('ref_axis',(-1.,0.,0.));
#19458=DIRECTION('',(0.,-1.,0.));
#19459=DIRECTION('',(0.,1.,0.));
#19460=DIRECTION('',(1.,0.,0.));
#19461=DIRECTION('center_axis',(0.,-1.,0.));
#19462=DIRECTION('ref_axis',(0.,0.,-1.));
#19463=DIRECTION('center_axis',(0.,-1.,0.));
#19464=DIRECTION('ref_axis',(1.,0.,0.));
#19465=DIRECTION('center_axis',(0.,1.,0.));
#19466=DIRECTION('ref_axis',(1.,0.,0.));
#19467=DIRECTION('',(-1.,0.,0.));
#19468=DIRECTION('center_axis',(0.,0.,1.));
#19469=DIRECTION('ref_axis',(1.,0.,0.));
#19470=DIRECTION('',(0.,1.,0.));
#19471=DIRECTION('',(0.,-1.,0.));
#19472=DIRECTION('center_axis',(0.,1.,0.));
#19473=DIRECTION('ref_axis',(0.,0.,1.));
#19474=DIRECTION('center_axis',(0.,-1.,0.));
#19475=DIRECTION('ref_axis',(1.,0.,0.));
#19476=DIRECTION('center_axis',(0.,-1.,0.));
#19477=DIRECTION('ref_axis',(1.,0.,0.));
#19478=DIRECTION('center_axis',(0.,-1.,0.));
#19479=DIRECTION('ref_axis',(1.,0.,0.));
#19480=DIRECTION('center_axis',(0.,-1.,0.));
#19481=DIRECTION('ref_axis',(1.,0.,0.));
#19482=DIRECTION('',(0.,1.,0.));
#19483=DIRECTION('center_axis',(0.,-1.,0.));
#19484=DIRECTION('ref_axis',(0.,0.,-1.));
#19485=DIRECTION('center_axis',(0.,-1.,0.));
#19486=DIRECTION('ref_axis',(1.,0.,0.));
#19487=DIRECTION('center_axis',(0.,-1.,0.));
#19488=DIRECTION('ref_axis',(1.,0.,0.));
#19489=DIRECTION('',(0.,1.,0.));
#19490=DIRECTION('',(0.,0.,1.));
#19491=DIRECTION('',(1.,0.,0.));
#19492=DIRECTION('',(0.,0.,1.));
#19493=DIRECTION('',(1.,0.,0.));
#19494=DIRECTION('axis',(0.,0.,1.));
#19495=DIRECTION('refdir',(1.,0.,0.));
#19496=DIRECTION('center_axis',(0.866025403784439,0.,-0.5));
#19497=DIRECTION('ref_axis',(0.5,0.,0.866025403784439));
#19498=DIRECTION('',(-0.5,0.,-0.866025403784439));
#19499=DIRECTION('',(0.,-1.,0.));
#19500=DIRECTION('',(0.5,0.,0.866025403784439));
#19501=DIRECTION('',(0.,-1.,0.));
#19502=DIRECTION('center_axis',(1.60246890531964E-16,0.,-1.));
#19503=DIRECTION('ref_axis',(1.,0.,1.60246890531964E-16));
#19504=DIRECTION('',(-1.,0.,-1.60246890531964E-16));
#19505=DIRECTION('',(0.,-1.,0.));
#19506=DIRECTION('',(1.,0.,1.60246890531964E-16));
#19507=DIRECTION('center_axis',(-0.866025403784439,0.,-0.5));
#19508=DIRECTION('ref_axis',(0.5,0.,-0.866025403784439));
#19509=DIRECTION('',(-0.5,0.,0.866025403784439));
#19510=DIRECTION('',(0.,-1.,0.));
#19511=DIRECTION('',(0.5,0.,-0.866025403784439));
#19512=DIRECTION('center_axis',(-0.866025403784439,0.,0.5));
#19513=DIRECTION('ref_axis',(-0.5,0.,-0.866025403784439));
#19514=DIRECTION('',(0.5,0.,0.866025403784439));
#19515=DIRECTION('',(0.,-1.,0.));
#19516=DIRECTION('',(-0.5,0.,-0.866025403784439));
#19517=DIRECTION('center_axis',(-1.60246890531964E-16,0.,1.));
#19518=DIRECTION('ref_axis',(-1.,0.,-1.60246890531964E-16));
#19519=DIRECTION('',(1.,0.,1.60246890531964E-16));
#19520=DIRECTION('',(0.,-1.,0.));
#19521=DIRECTION('',(-1.,0.,-1.60246890531964E-16));
#19522=DIRECTION('center_axis',(0.866025403784439,0.,0.5));
#19523=DIRECTION('ref_axis',(-0.5,0.,0.866025403784439));
#19524=DIRECTION('',(0.5,0.,-0.866025403784439));
#19525=DIRECTION('',(-0.5,0.,0.866025403784439));
#19526=DIRECTION('center_axis',(0.,1.,0.));
#19527=DIRECTION('ref_axis',(1.,0.,0.));
#19528=DIRECTION('center_axis',(0.,-1.,0.));
#19529=DIRECTION('ref_axis',(0.,0.,-1.));
#19530=DIRECTION('center_axis',(0.,1.,0.));
#19531=DIRECTION('ref_axis',(1.,0.,0.));
#19532=DIRECTION('center_axis',(0.,1.,0.));
#19533=DIRECTION('ref_axis',(1.,0.,0.));
#19534=DIRECTION('center_axis',(0.,1.,0.));
#19535=DIRECTION('ref_axis',(0.,0.,1.));
#19536=DIRECTION('center_axis',(0.,-1.,0.));
#19537=DIRECTION('ref_axis',(1.,0.,0.));
#19538=DIRECTION('center_axis',(0.,-1.,0.));
#19539=DIRECTION('ref_axis',(1.,0.,0.));
#19540=DIRECTION('center_axis',(0.,-1.,0.));
#19541=DIRECTION('ref_axis',(1.,0.,0.));
#19542=DIRECTION('',(0.707106781186547,0.707106781186548,8.65956056235493E-17));
#19543=DIRECTION('center_axis',(0.,-1.,0.));
#19544=DIRECTION('ref_axis',(1.,0.,0.));
#19545=DIRECTION('center_axis',(0.,-1.,0.));
#19546=DIRECTION('ref_axis',(1.,0.,0.));
#19547=DIRECTION('',(0.,1.,0.));
#19548=DIRECTION('center_axis',(0.,1.,0.));
#19549=DIRECTION('ref_axis',(1.,0.,0.));
#19550=DIRECTION('center_axis',(0.,-1.,0.));
#19551=DIRECTION('ref_axis',(1.,0.,0.));
#19552=DIRECTION('',(-0.707106781186547,0.707106781186548,-8.65956056235493E-17));
#19553=DIRECTION('center_axis',(0.,-1.,0.));
#19554=DIRECTION('ref_axis',(0.,0.,-1.));
#19555=DIRECTION('center_axis',(0.,-1.,0.));
#19556=DIRECTION('ref_axis',(1.,0.,0.));
#19557=DIRECTION('center_axis',(0.,1.,0.));
#19558=DIRECTION('ref_axis',(1.,0.,0.));
#19559=DIRECTION('center_axis',(0.,1.,0.));
#19560=DIRECTION('ref_axis',(1.,0.,0.));
#19561=DIRECTION('',(-0.447213595499958,0.894427190999916,-5.47678698264203E-17));
#19562=DIRECTION('center_axis',(0.,-1.,0.));
#19563=DIRECTION('ref_axis',(1.,0.,0.));
#19564=DIRECTION('',(0.,1.,0.));
#19565=DIRECTION('',(0.,0.,1.));
#19566=DIRECTION('',(1.,0.,0.));
#19567=DIRECTION('',(0.,0.,1.));
#19568=DIRECTION('',(1.,0.,0.));
#19569=DIRECTION('',(0.,0.,1.));
#19570=DIRECTION('',(1.,0.,0.));
#19571=DIRECTION('',(0.,0.,1.));
#19572=DIRECTION('',(1.,0.,0.));
#19573=DIRECTION('',(0.,0.,1.));
#19574=DIRECTION('',(1.,0.,0.));
#19575=DIRECTION('',(0.,0.,1.));
#19576=DIRECTION('',(1.,0.,0.));
#19577=DIRECTION('',(0.,0.,1.));
#19578=DIRECTION('',(1.,0.,0.));
#19579=DIRECTION('',(0.,0.,1.));
#19580=DIRECTION('',(2.22044604925031E-16,-1.,0.));
#19581=DIRECTION('',(0.,0.,1.));
#19582=DIRECTION('',(2.22044604925031E-16,-1.,0.));
#19583=DIRECTION('',(0.,0.,1.));
#19584=DIRECTION('',(1.,0.,0.));
#19585=DIRECTION('axis',(0.,0.,1.));
#19586=DIRECTION('refdir',(1.,0.,0.));
#19587=DIRECTION('axis',(0.,0.,1.));
#19588=DIRECTION('refdir',(1.,0.,0.));
#19589=DIRECTION('center_axis',(0.,1.,0.));
#19590=DIRECTION('ref_axis',(1.,0.,0.));
#19591=DIRECTION('center_axis',(0.,1.,0.));
#19592=DIRECTION('ref_axis',(1.,0.,0.));
#19593=DIRECTION('',(0.,1.,0.));
#19594=DIRECTION('center_axis',(0.,-1.,0.));
#19595=DIRECTION('ref_axis',(1.,0.,0.));
#19596=DIRECTION('center_axis',(0.,1.,0.));
#19597=DIRECTION('ref_axis',(1.,0.,0.));
#19598=DIRECTION('',(0.,-1.,0.));
#19599=DIRECTION('center_axis',(0.,1.,0.));
#19600=DIRECTION('ref_axis',(1.,0.,0.));
#19601=DIRECTION('',(0.,1.,0.));
#19602=DIRECTION('center_axis',(0.,1.,0.));
#19603=DIRECTION('ref_axis',(1.,0.,0.));
#19604=DIRECTION('center_axis',(0.,1.,0.));
#19605=DIRECTION('ref_axis',(1.,0.,0.));
#19606=DIRECTION('',(0.874781243901175,0.,0.484518085646669));
#19607=DIRECTION('center_axis',(0.,1.,0.));
#19608=DIRECTION('ref_axis',(1.,0.,0.));
#19609=DIRECTION('',(-0.874781243901175,0.,-0.484518085646669));
#19610=DIRECTION('center_axis',(0.,1.,0.));
#19611=DIRECTION('ref_axis',(1.,0.,0.));
#19612=DIRECTION('center_axis',(-0.484518085646669,0.,0.874781243901175));
#19613=DIRECTION('ref_axis',(0.874781243901175,0.,0.484518085646669));
#19614=DIRECTION('',(0.874781243901175,0.,0.484518085646669));
#19615=DIRECTION('',(0.,-1.,0.));
#19616=DIRECTION('center_axis',(0.,1.,0.));
#19617=DIRECTION('ref_axis',(1.,0.,0.));
#19618=DIRECTION('',(0.,1.,0.));
#19619=DIRECTION('center_axis',(0.,-1.,0.));
#19620=DIRECTION('ref_axis',(1.,0.,0.));
#19621=DIRECTION('center_axis',(0.,1.,0.));
#19622=DIRECTION('ref_axis',(-0.874781243901175,0.,-0.48451808564667));
#19623=DIRECTION('',(0.,1.,0.));
#19624=DIRECTION('center_axis',(0.,1.,0.));
#19625=DIRECTION('ref_axis',(1.,0.,0.));
#19626=DIRECTION('center_axis',(0.484518085646669,0.,-0.874781243901175));
#19627=DIRECTION('ref_axis',(-0.874781243901175,0.,-0.484518085646669));
#19628=DIRECTION('',(-0.874781243901175,0.,-0.484518085646669));
#19629=DIRECTION('center_axis',(0.,1.,0.));
#19630=DIRECTION('ref_axis',(0.,0.,1.));
#19631=DIRECTION('',(0.,0.,1.));
#19632=DIRECTION('',(1.,0.,0.));
#19633=DIRECTION('axis',(0.,0.,1.));
#19634=DIRECTION('refdir',(1.,0.,0.));
#19635=DIRECTION('axis',(0.,0.,1.));
#19636=DIRECTION('refdir',(1.,0.,0.));
#19637=DIRECTION('center_axis',(1.,0.,0.));
#19638=DIRECTION('ref_axis',(0.,0.,-1.));
#19639=DIRECTION('center_axis',(1.,0.,0.));
#19640=DIRECTION('ref_axis',(0.,0.,-1.));
#19641=DIRECTION('',(-1.,0.,0.));
#19642=DIRECTION('center_axis',(1.,0.,0.));
#19643=DIRECTION('ref_axis',(0.,0.,-1.));
#19644=DIRECTION('center_axis',(1.,0.,0.));
#19645=DIRECTION('ref_axis',(0.,0.,-1.));
#19646=DIRECTION('center_axis',(1.,0.,0.));
#19647=DIRECTION('ref_axis',(0.,0.,-1.));
#19648=DIRECTION('axis',(0.,0.,1.));
#19649=DIRECTION('refdir',(1.,0.,0.));
#19650=DIRECTION('center_axis',(1.,0.,0.));
#19651=DIRECTION('ref_axis',(0.,0.,-1.));
#19652=DIRECTION('center_axis',(-1.,0.,0.));
#19653=DIRECTION('ref_axis',(0.,0.,-1.));
#19654=DIRECTION('',(-1.,0.,0.));
#19655=DIRECTION('center_axis',(-1.,0.,0.));
#19656=DIRECTION('ref_axis',(0.,0.,-1.));
#19657=DIRECTION('center_axis',(1.,0.,0.));
#19658=DIRECTION('ref_axis',(0.,0.,-1.));
#19659=DIRECTION('center_axis',(1.,0.,0.));
#19660=DIRECTION('ref_axis',(0.,0.,-1.));
#19661=DIRECTION('',(-1.,0.,0.));
#19662=DIRECTION('center_axis',(1.,0.,0.));
#19663=DIRECTION('ref_axis',(0.,0.,-1.));
#19664=DIRECTION('center_axis',(1.,0.,0.));
#19665=DIRECTION('ref_axis',(0.,0.,-1.));
#19666=DIRECTION('center_axis',(1.,0.,0.));
#19667=DIRECTION('ref_axis',(0.,0.,-1.));
#19668=DIRECTION('axis',(0.,0.,1.));
#19669=DIRECTION('refdir',(1.,0.,0.));
#19670=DIRECTION('center_axis',(1.,0.,0.));
#19671=DIRECTION('ref_axis',(0.,0.,-1.));
#19672=DIRECTION('center_axis',(-1.,0.,0.));
#19673=DIRECTION('ref_axis',(0.,0.,-1.));
#19674=DIRECTION('',(-1.,0.,0.));
#19675=DIRECTION('center_axis',(-1.,0.,0.));
#19676=DIRECTION('ref_axis',(0.,0.,-1.));
#19677=DIRECTION('center_axis',(1.,0.,0.));
#19678=DIRECTION('ref_axis',(0.,0.,-1.));
#19679=DIRECTION('center_axis',(1.,0.,0.));
#19680=DIRECTION('ref_axis',(0.,0.,-1.));
#19681=DIRECTION('',(-1.,0.,0.));
#19682=DIRECTION('center_axis',(1.,0.,0.));
#19683=DIRECTION('ref_axis',(0.,0.,-1.));
#19684=DIRECTION('center_axis',(1.,0.,0.));
#19685=DIRECTION('ref_axis',(0.,0.,-1.));
#19686=DIRECTION('center_axis',(1.,0.,0.));
#19687=DIRECTION('ref_axis',(0.,0.,-1.));
#19688=DIRECTION('axis',(0.,0.,1.));
#19689=DIRECTION('refdir',(1.,0.,0.));
#19690=DIRECTION('center_axis',(1.,0.,0.));
#19691=DIRECTION('ref_axis',(0.,0.,-1.));
#19692=DIRECTION('center_axis',(-1.,0.,0.));
#19693=DIRECTION('ref_axis',(0.,0.,-1.));
#19694=DIRECTION('',(-1.,0.,0.));
#19695=DIRECTION('center_axis',(-1.,0.,0.));
#19696=DIRECTION('ref_axis',(0.,0.,-1.));
#19697=DIRECTION('center_axis',(1.,0.,0.));
#19698=DIRECTION('ref_axis',(0.,0.,-1.));
#19699=DIRECTION('center_axis',(1.,0.,0.));
#19700=DIRECTION('ref_axis',(0.,0.,-1.));
#19701=DIRECTION('',(-1.,0.,0.));
#19702=DIRECTION('center_axis',(1.,0.,0.));
#19703=DIRECTION('ref_axis',(0.,0.,-1.));
#19704=DIRECTION('center_axis',(1.,0.,0.));
#19705=DIRECTION('ref_axis',(0.,0.,-1.));
#19706=DIRECTION('center_axis',(1.,0.,0.));
#19707=DIRECTION('ref_axis',(0.,0.,-1.));
#19708=DIRECTION('axis',(0.,0.,1.));
#19709=DIRECTION('refdir',(1.,0.,0.));
#19710=DIRECTION('center_axis',(1.,0.,0.));
#19711=DIRECTION('ref_axis',(0.,0.,-1.));
#19712=DIRECTION('center_axis',(1.,0.,0.));
#19713=DIRECTION('ref_axis',(0.,0.,-1.));
#19714=DIRECTION('',(-1.,0.,0.));
#19715=DIRECTION('center_axis',(1.,0.,0.));
#19716=DIRECTION('ref_axis',(0.,0.,-1.));
#19717=DIRECTION('center_axis',(1.,0.,0.));
#19718=DIRECTION('ref_axis',(0.,0.,-1.));
#19719=DIRECTION('center_axis',(1.,0.,0.));
#19720=DIRECTION('ref_axis',(0.,0.,-1.));
#19721=DIRECTION('',(0.,0.,1.));
#19722=DIRECTION('',(1.,0.,0.));
#19723=DIRECTION('',(0.,0.,1.));
#19724=DIRECTION('',(1.,0.,0.));
#19725=DIRECTION('',(0.,0.,1.));
#19726=DIRECTION('',(1.,0.,0.));
#19727=DIRECTION('',(0.,0.,1.));
#19728=DIRECTION('',(1.,0.,0.));
#19729=DIRECTION('',(0.,0.,1.));
#19730=DIRECTION('',(1.,0.,0.));
#19731=DIRECTION('',(0.,0.,1.));
#19732=DIRECTION('',(1.,0.,0.));
#19733=DIRECTION('',(0.,0.,1.));
#19734=DIRECTION('',(1.,0.,0.));
#19735=DIRECTION('',(0.,0.,1.));
#19736=DIRECTION('',(1.,0.,0.));
#19737=DIRECTION('',(0.,0.,1.));
#19738=DIRECTION('',(1.,0.,0.));
#19739=DIRECTION('',(0.,0.,1.));
#19740=DIRECTION('',(1.,0.,0.));
#19741=DIRECTION('',(0.,0.,1.));
#19742=DIRECTION('',(1.,0.,0.));
#19743=DIRECTION('',(0.,0.,1.));
#19744=DIRECTION('',(1.,0.,0.));
#19745=CARTESIAN_POINT('',(0.,0.,0.));
#19746=CARTESIAN_POINT('',(0.,0.,0.));
#19747=CARTESIAN_POINT('',(0.,0.,0.));
#19748=CARTESIAN_POINT('Origin',(0.5,-0.8,-0.1));
#19749=CARTESIAN_POINT('',(0.335,-0.8,0.));
#19750=CARTESIAN_POINT('Origin',(0.5,-0.8,0.));
#19751=CARTESIAN_POINT('',(0.335,-0.8,1.));
#19752=CARTESIAN_POINT('',(0.335,-0.8,-0.1));
#19753=CARTESIAN_POINT('Origin',(0.5,-0.8,1.));
#19754=CARTESIAN_POINT('Origin',(0.5,-8.2,-0.1));
#19755=CARTESIAN_POINT('',(0.335,-8.2,0.));
#19756=CARTESIAN_POINT('Origin',(0.5,-8.2,0.));
#19757=CARTESIAN_POINT('',(0.335,-8.2,1.));
#19758=CARTESIAN_POINT('',(0.335,-8.2,-0.1));
#19759=CARTESIAN_POINT('Origin',(0.5,-8.2,1.));
#19760=CARTESIAN_POINT('Origin',(-9.5,-0.8,-0.1));
#19761=CARTESIAN_POINT('',(-9.665,-0.8,0.));
#19762=CARTESIAN_POINT('Origin',(-9.5,-0.8,0.));
#19763=CARTESIAN_POINT('',(-9.665,-0.8,1.));
#19764=CARTESIAN_POINT('',(-9.665,-0.8,-0.1));
#19765=CARTESIAN_POINT('Origin',(-9.5,-0.8,1.));
#19766=CARTESIAN_POINT('Origin',(-9.5,-8.2,-0.1));
#19767=CARTESIAN_POINT('',(-9.665,-8.2,0.));
#19768=CARTESIAN_POINT('Origin',(-9.5,-8.2,0.));
#19769=CARTESIAN_POINT('',(-9.665,-8.2,1.));
#19770=CARTESIAN_POINT('',(-9.665,-8.2,-0.1));
#19771=CARTESIAN_POINT('Origin',(-9.5,-8.2,1.));
#19772=CARTESIAN_POINT('Origin',(21.2,7.8,-0.1));
#19773=CARTESIAN_POINT('',(20.99,7.8,0.));
#19774=CARTESIAN_POINT('Origin',(21.2,7.8,0.));
#19775=CARTESIAN_POINT('',(20.99,7.8,1.));
#19776=CARTESIAN_POINT('',(20.99,7.8,-0.1));
#19777=CARTESIAN_POINT('Origin',(21.2,7.8,1.));
#19778=CARTESIAN_POINT('Origin',(21.2,5.2,-0.1));
#19779=CARTESIAN_POINT('',(20.99,5.2,0.));
#19780=CARTESIAN_POINT('Origin',(21.2,5.2,0.));
#19781=CARTESIAN_POINT('',(20.99,5.2,1.));
#19782=CARTESIAN_POINT('',(20.99,5.2,-0.1));
#19783=CARTESIAN_POINT('Origin',(21.2,5.2,1.));
#19784=CARTESIAN_POINT('Origin',(14.8,7.8,-0.1));
#19785=CARTESIAN_POINT('',(14.59,7.8,0.));
#19786=CARTESIAN_POINT('Origin',(14.8,7.8,0.));
#19787=CARTESIAN_POINT('',(14.59,7.8,1.));
#19788=CARTESIAN_POINT('',(14.59,7.8,-0.1));
#19789=CARTESIAN_POINT('Origin',(14.8,7.8,1.));
#19790=CARTESIAN_POINT('Origin',(14.8,5.2,-0.1));
#19791=CARTESIAN_POINT('',(14.59,5.2,0.));
#19792=CARTESIAN_POINT('Origin',(14.8,5.2,0.));
#19793=CARTESIAN_POINT('',(14.59,5.2,1.));
#19794=CARTESIAN_POINT('',(14.59,5.2,-0.1));
#19795=CARTESIAN_POINT('Origin',(14.8,5.2,1.));
#19796=CARTESIAN_POINT('Origin',(3.2,7.8,-0.1));
#19797=CARTESIAN_POINT('',(2.99,7.8,0.));
#19798=CARTESIAN_POINT('Origin',(3.2,7.8,0.));
#19799=CARTESIAN_POINT('',(2.99,7.8,1.));
#19800=CARTESIAN_POINT('',(2.99,7.8,-0.1));
#19801=CARTESIAN_POINT('Origin',(3.2,7.8,1.));
#19802=CARTESIAN_POINT('Origin',(3.2,5.2,-0.1));
#19803=CARTESIAN_POINT('',(2.99,5.2,0.));
#19804=CARTESIAN_POINT('Origin',(3.2,5.2,0.));
#19805=CARTESIAN_POINT('',(2.99,5.2,1.));
#19806=CARTESIAN_POINT('',(2.99,5.2,-0.1));
#19807=CARTESIAN_POINT('Origin',(3.2,5.2,1.));
#19808=CARTESIAN_POINT('Origin',(-3.2,7.8,-0.1));
#19809=CARTESIAN_POINT('',(-3.41,7.8,0.));
#19810=CARTESIAN_POINT('Origin',(-3.2,7.8,0.));
#19811=CARTESIAN_POINT('',(-3.41,7.8,1.));
#19812=CARTESIAN_POINT('',(-3.41,7.8,-0.1));
#19813=CARTESIAN_POINT('Origin',(-3.2,7.8,1.));
#19814=CARTESIAN_POINT('Origin',(-3.2,5.2,-0.1));
#19815=CARTESIAN_POINT('',(-3.41,5.2,0.));
#19816=CARTESIAN_POINT('Origin',(-3.2,5.2,0.));
#19817=CARTESIAN_POINT('',(-3.41,5.2,1.));
#19818=CARTESIAN_POINT('',(-3.41,5.2,-0.1));
#19819=CARTESIAN_POINT('Origin',(-3.2,5.2,1.));
#19820=CARTESIAN_POINT('Origin',(31.,10.,0.));
#19821=CARTESIAN_POINT('',(31.,10.,0.));
#19822=CARTESIAN_POINT('',(-14.,10.,0.));
#19823=CARTESIAN_POINT('',(31.,10.,0.));
#19824=CARTESIAN_POINT('',(-14.,10.,1.));
#19825=CARTESIAN_POINT('',(-14.,10.,0.));
#19826=CARTESIAN_POINT('',(31.,10.,1.));
#19827=CARTESIAN_POINT('',(31.,10.,1.));
#19828=CARTESIAN_POINT('',(31.,10.,0.));
#19829=CARTESIAN_POINT('Origin',(31.,-10.,0.));
#19830=CARTESIAN_POINT('',(31.,-10.,0.));
#19831=CARTESIAN_POINT('',(31.,-10.,0.));
#19832=CARTESIAN_POINT('',(31.,-10.,1.));
#19833=CARTESIAN_POINT('',(31.,-10.,1.));
#19834=CARTESIAN_POINT('',(31.,-10.,0.));
#19835=CARTESIAN_POINT('Origin',(-14.,-10.,0.));
#19836=CARTESIAN_POINT('',(-14.,-10.,0.));
#19837=CARTESIAN_POINT('',(-14.,-10.,0.));
#19838=CARTESIAN_POINT('',(-14.,-10.,1.));
#19839=CARTESIAN_POINT('',(-14.,-10.,1.));
#19840=CARTESIAN_POINT('',(-14.,-10.,0.));
#19841=CARTESIAN_POINT('Origin',(-14.,10.,0.));
#19842=CARTESIAN_POINT('',(-14.,10.,0.));
#19843=CARTESIAN_POINT('',(-14.,10.,1.));
#19844=CARTESIAN_POINT('Origin',(8.5,0.,1.));
#19845=CARTESIAN_POINT('Origin',(8.5,0.,0.));
#19846=CARTESIAN_POINT('',(0.,0.,0.));
#19847=CARTESIAN_POINT('Origin',(-13.,10.,-0.8));
#19848=CARTESIAN_POINT('',(-13.,10.,-0.8));
#19849=CARTESIAN_POINT('',(-14.,10.,-0.8));
#19850=CARTESIAN_POINT('',(-13.,10.,-0.8));
#19851=CARTESIAN_POINT('',(-14.,10.,0.));
#19852=CARTESIAN_POINT('',(-14.,10.,-0.8));
#19853=CARTESIAN_POINT('',(-13.,10.,0.));
#19854=CARTESIAN_POINT('',(-13.,10.,0.));
#19855=CARTESIAN_POINT('',(-13.,10.,-0.8));
#19856=CARTESIAN_POINT('Origin',(-13.,-10.,-0.8));
#19857=CARTESIAN_POINT('',(-13.,-10.,-0.8));
#19858=CARTESIAN_POINT('',(-13.,-10.,-0.8));
#19859=CARTESIAN_POINT('',(-13.,-10.,0.));
#19860=CARTESIAN_POINT('',(-13.,-10.,0.));
#19861=CARTESIAN_POINT('',(-13.,-10.,-0.8));
#19862=CARTESIAN_POINT('Origin',(-14.,-10.,-0.8));
#19863=CARTESIAN_POINT('',(-14.,-10.,-0.8));
#19864=CARTESIAN_POINT('',(-14.,-10.,-0.8));
#19865=CARTESIAN_POINT('',(-14.,-10.,0.));
#19866=CARTESIAN_POINT('',(-14.,-10.,0.));
#19867=CARTESIAN_POINT('',(-14.,-10.,-0.8));
#19868=CARTESIAN_POINT('Origin',(-14.,10.,-0.8));
#19869=CARTESIAN_POINT('',(-14.,10.,-0.8));
#19870=CARTESIAN_POINT('',(-14.,10.,0.));
#19871=CARTESIAN_POINT('Origin',(-13.5,0.,0.));
#19872=CARTESIAN_POINT('Origin',(-13.5,0.,-0.8));
#19873=CARTESIAN_POINT('',(0.,0.,0.));
#19874=CARTESIAN_POINT('Origin',(31.,10.,-0.8));
#19875=CARTESIAN_POINT('',(31.,10.,-0.8));
#19876=CARTESIAN_POINT('',(30.,10.,-0.8));
#19877=CARTESIAN_POINT('',(31.,10.,-0.8));
#19878=CARTESIAN_POINT('',(30.,10.,0.));
#19879=CARTESIAN_POINT('',(30.,10.,-0.8));
#19880=CARTESIAN_POINT('',(31.,10.,0.));
#19881=CARTESIAN_POINT('',(31.,10.,0.));
#19882=CARTESIAN_POINT('',(31.,10.,-0.8));
#19883=CARTESIAN_POINT('Origin',(31.,-10.,-0.8));
#19884=CARTESIAN_POINT('',(31.,-10.,-0.8));
#19885=CARTESIAN_POINT('',(31.,-10.,-0.8));
#19886=CARTESIAN_POINT('',(31.,-10.,0.));
#19887=CARTESIAN_POINT('',(31.,-10.,0.));
#19888=CARTESIAN_POINT('',(31.,-10.,-0.8));
#19889=CARTESIAN_POINT('Origin',(30.,-10.,-0.8));
#19890=CARTESIAN_POINT('',(30.,-10.,-0.8));
#19891=CARTESIAN_POINT('',(30.,-10.,-0.8));
#19892=CARTESIAN_POINT('',(30.,-10.,0.));
#19893=CARTESIAN_POINT('',(30.,-10.,0.));
#19894=CARTESIAN_POINT('',(30.,-10.,-0.8));
#19895=CARTESIAN_POINT('Origin',(30.,10.,-0.8));
#19896=CARTESIAN_POINT('',(30.,10.,-0.8));
#19897=CARTESIAN_POINT('',(30.,10.,0.));
#19898=CARTESIAN_POINT('Origin',(30.5,0.,0.));
#19899=CARTESIAN_POINT('Origin',(30.5,0.,-0.8));
#19900=CARTESIAN_POINT('',(0.,0.,0.));
#19901=CARTESIAN_POINT('Origin',(1.15,4.4,15.));
#19902=CARTESIAN_POINT('',(0.985,4.5,15.));
#19903=CARTESIAN_POINT('Origin',(1.15,4.5,15.));
#19904=CARTESIAN_POINT('',(0.985,5.5,15.));
#19905=CARTESIAN_POINT('',(0.985,4.4,15.));
#19906=CARTESIAN_POINT('Origin',(1.15,5.5,15.));
#19907=CARTESIAN_POINT('Origin',(-0.575,4.4,15.9959292143521));
#19908=CARTESIAN_POINT('',(-0.74,4.5,15.9959292143521));
#19909=CARTESIAN_POINT('Origin',(-0.575,4.5,15.9959292143521));
#19910=CARTESIAN_POINT('',(-0.74,5.5,15.9959292143521));
#19911=CARTESIAN_POINT('',(-0.74,4.4,15.9959292143521));
#19912=CARTESIAN_POINT('Origin',(-0.575,5.5,15.9959292143521));
#19913=CARTESIAN_POINT('Origin',(-0.575000000000001,4.4,14.0040707856479));
#19914=CARTESIAN_POINT('',(-0.74,4.5,14.0040707856479));
#19915=CARTESIAN_POINT('Origin',(-0.575000000000001,4.5,14.0040707856479));
#19916=CARTESIAN_POINT('',(-0.74,5.5,14.0040707856479));
#19917=CARTESIAN_POINT('',(-0.74,4.4,14.0040707856479));
#19918=CARTESIAN_POINT('Origin',(-0.575000000000001,5.5,14.0040707856479));
#19919=CARTESIAN_POINT('Origin',(0.,4.4,15.));
#19920=CARTESIAN_POINT('',(-0.605,4.5,15.));
#19921=CARTESIAN_POINT('Origin',(0.,4.5,15.));
#19922=CARTESIAN_POINT('',(-0.605,5.5,15.));
#19923=CARTESIAN_POINT('',(-0.605,4.4,15.));
#19924=CARTESIAN_POINT('Origin',(0.,5.5,15.));
#19925=CARTESIAN_POINT('Origin',(3.2,7.8,0.9));
#19926=CARTESIAN_POINT('',(2.925,7.8,1.));
#19927=CARTESIAN_POINT('Origin',(3.2,7.8,1.));
#19928=CARTESIAN_POINT('',(2.925,7.8,1.8));
#19929=CARTESIAN_POINT('',(2.925,7.8,0.9));
#19930=CARTESIAN_POINT('Origin',(3.2,7.8,1.8));
#19931=CARTESIAN_POINT('Origin',(3.2,5.2,0.9));
#19932=CARTESIAN_POINT('',(2.925,5.2,1.));
#19933=CARTESIAN_POINT('Origin',(3.2,5.2,1.));
#19934=CARTESIAN_POINT('',(2.925,5.2,1.8));
#19935=CARTESIAN_POINT('',(2.925,5.2,0.9));
#19936=CARTESIAN_POINT('Origin',(3.2,5.2,1.8));
#19937=CARTESIAN_POINT('Origin',(-3.2,7.8,0.9));
#19938=CARTESIAN_POINT('',(-3.475,7.8,1.));
#19939=CARTESIAN_POINT('Origin',(-3.2,7.8,1.));
#19940=CARTESIAN_POINT('',(-3.475,7.8,1.8));
#19941=CARTESIAN_POINT('',(-3.475,7.8,0.9));
#19942=CARTESIAN_POINT('Origin',(-3.2,7.8,1.8));
#19943=CARTESIAN_POINT('Origin',(-3.2,5.2,0.9));
#19944=CARTESIAN_POINT('',(-3.475,5.2,1.));
#19945=CARTESIAN_POINT('Origin',(-3.2,5.2,1.));
#19946=CARTESIAN_POINT('',(-3.475,5.2,1.8));
#19947=CARTESIAN_POINT('',(-3.475,5.2,0.9));
#19948=CARTESIAN_POINT('Origin',(-3.2,5.2,1.8));
#19949=CARTESIAN_POINT('Origin',(-4.,4.5,1.8));
#19950=CARTESIAN_POINT('',(-2.5,5.5,1.8));
#19951=CARTESIAN_POINT('',(-2.5,4.5,1.8));
#19952=CARTESIAN_POINT('',(-2.5,5.,1.8));
#19953=CARTESIAN_POINT('',(2.5,5.5,1.8));
#19954=CARTESIAN_POINT('',(-0.75,5.5,1.8));
#19955=CARTESIAN_POINT('',(2.5,4.5,1.8));
#19956=CARTESIAN_POINT('',(2.5,4.5,1.8));
#19957=CARTESIAN_POINT('',(4.,4.5,1.8));
#19958=CARTESIAN_POINT('',(4.,4.5,1.8));
#19959=CARTESIAN_POINT('',(4.,8.5,1.8));
#19960=CARTESIAN_POINT('',(4.,4.5,1.8));
#19961=CARTESIAN_POINT('',(-4.,8.5,1.8));
#19962=CARTESIAN_POINT('',(4.,8.5,1.8));
#19963=CARTESIAN_POINT('',(-4.,4.5,1.8));
#19964=CARTESIAN_POINT('',(-4.,4.5,1.8));
#19965=CARTESIAN_POINT('',(4.,4.5,1.8));
#19966=CARTESIAN_POINT('Origin',(-4.,4.5,1.));
#19967=CARTESIAN_POINT('',(-4.,4.5,1.));
#19968=CARTESIAN_POINT('',(-4.,4.5,1.8));
#19969=CARTESIAN_POINT('',(-4.,8.5,1.));
#19970=CARTESIAN_POINT('',(-4.,8.5,1.8));
#19971=CARTESIAN_POINT('',(-4.,4.5,1.));
#19972=CARTESIAN_POINT('Origin',(4.,4.5,1.8));
#19973=CARTESIAN_POINT('',(4.,4.5,1.));
#19974=CARTESIAN_POINT('',(4.,4.5,1.));
#19975=CARTESIAN_POINT('',(4.,8.5,1.));
#19976=CARTESIAN_POINT('',(4.,4.5,1.));
#19977=CARTESIAN_POINT('',(4.,8.5,1.));
#19978=CARTESIAN_POINT('Origin',(0.,8.5,1.4));
#19979=CARTESIAN_POINT('',(-4.,8.5,1.));
#19980=CARTESIAN_POINT('Origin',(-2.5,4.5,1.));
#19981=CARTESIAN_POINT('',(2.5,4.5,18.));
#19982=CARTESIAN_POINT('',(2.5,4.5,1.));
#19983=CARTESIAN_POINT('',(-2.5,4.5,18.));
#19984=CARTESIAN_POINT('',(-2.5,4.5,18.));
#19985=CARTESIAN_POINT('',(-2.5,4.5,1.));
#19986=CARTESIAN_POINT('',(-4.,4.5,1.));
#19987=CARTESIAN_POINT('Origin',(2.5,4.5,1.));
#19988=CARTESIAN_POINT('',(2.5,5.5,18.));
#19989=CARTESIAN_POINT('',(2.5,5.5,1.));
#19990=CARTESIAN_POINT('',(2.5,4.5,18.));
#19991=CARTESIAN_POINT('Origin',(2.5,5.5,1.));
#19992=CARTESIAN_POINT('',(-2.5,5.5,18.));
#19993=CARTESIAN_POINT('',(-2.5,5.5,1.));
#19994=CARTESIAN_POINT('',(2.5,5.5,18.));
#19995=CARTESIAN_POINT('Origin',(-2.5,5.5,1.));
#19996=CARTESIAN_POINT('',(-2.5,5.5,18.));
#19997=CARTESIAN_POINT('Origin',(0.,5.,18.));
#19998=CARTESIAN_POINT('Origin',(0.,5.,1.));
#19999=CARTESIAN_POINT('',(0.,0.,0.));
#20000=CARTESIAN_POINT('Origin',(19.15,4.4,15.));
#20001=CARTESIAN_POINT('',(18.985,4.5,15.));
#20002=CARTESIAN_POINT('Origin',(19.15,4.5,15.));
#20003=CARTESIAN_POINT('',(18.985,5.5,15.));
#20004=CARTESIAN_POINT('',(18.985,4.4,15.));
#20005=CARTESIAN_POINT('Origin',(19.15,5.5,15.));
#20006=CARTESIAN_POINT('Origin',(17.425,4.4,15.9959292143521));
#20007=CARTESIAN_POINT('',(17.26,4.5,15.9959292143521));
#20008=CARTESIAN_POINT('Origin',(17.425,4.5,15.9959292143521));
#20009=CARTESIAN_POINT('',(17.26,5.5,15.9959292143521));
#20010=CARTESIAN_POINT('',(17.26,4.4,15.9959292143521));
#20011=CARTESIAN_POINT('Origin',(17.425,5.5,15.9959292143521));
#20012=CARTESIAN_POINT('Origin',(17.425,4.4,14.0040707856479));
#20013=CARTESIAN_POINT('',(17.26,4.5,14.0040707856479));
#20014=CARTESIAN_POINT('Origin',(17.425,4.5,14.0040707856479));
#20015=CARTESIAN_POINT('',(17.26,5.5,14.0040707856479));
#20016=CARTESIAN_POINT('',(17.26,4.4,14.0040707856479));
#20017=CARTESIAN_POINT('Origin',(17.425,5.5,14.0040707856479));
#20018=CARTESIAN_POINT('Origin',(18.,4.4,15.));
#20019=CARTESIAN_POINT('',(17.395,4.5,15.));
#20020=CARTESIAN_POINT('Origin',(18.,4.5,15.));
#20021=CARTESIAN_POINT('',(17.395,5.5,15.));
#20022=CARTESIAN_POINT('',(17.395,4.4,15.));
#20023=CARTESIAN_POINT('Origin',(18.,5.5,15.));
#20024=CARTESIAN_POINT('Origin',(21.2,7.8,0.9));
#20025=CARTESIAN_POINT('',(20.925,7.8,1.));
#20026=CARTESIAN_POINT('Origin',(21.2,7.8,1.));
#20027=CARTESIAN_POINT('',(20.925,7.8,1.8));
#20028=CARTESIAN_POINT('',(20.925,7.8,0.9));
#20029=CARTESIAN_POINT('Origin',(21.2,7.8,1.8));
#20030=CARTESIAN_POINT('Origin',(21.2,5.2,0.9));
#20031=CARTESIAN_POINT('',(20.925,5.2,1.));
#20032=CARTESIAN_POINT('Origin',(21.2,5.2,1.));
#20033=CARTESIAN_POINT('',(20.925,5.2,1.8));
#20034=CARTESIAN_POINT('',(20.925,5.2,0.9));
#20035=CARTESIAN_POINT('Origin',(21.2,5.2,1.8));
#20036=CARTESIAN_POINT('Origin',(14.8,7.8,0.9));
#20037=CARTESIAN_POINT('',(14.525,7.8,1.));
#20038=CARTESIAN_POINT('Origin',(14.8,7.8,1.));
#20039=CARTESIAN_POINT('',(14.525,7.8,1.8));
#20040=CARTESIAN_POINT('',(14.525,7.8,0.9));
#20041=CARTESIAN_POINT('Origin',(14.8,7.8,1.8));
#20042=CARTESIAN_POINT('Origin',(14.8,5.2,0.9));
#20043=CARTESIAN_POINT('',(14.525,5.2,1.));
#20044=CARTESIAN_POINT('Origin',(14.8,5.2,1.));
#20045=CARTESIAN_POINT('',(14.525,5.2,1.8));
#20046=CARTESIAN_POINT('',(14.525,5.2,0.9));
#20047=CARTESIAN_POINT('Origin',(14.8,5.2,1.8));
#20048=CARTESIAN_POINT('Origin',(14.,4.5,1.8));
#20049=CARTESIAN_POINT('',(15.5,5.5,1.8));
#20050=CARTESIAN_POINT('',(15.5,4.5,1.8));
#20051=CARTESIAN_POINT('',(15.5,5.,1.8));
#20052=CARTESIAN_POINT('',(20.5,5.5,1.8));
#20053=CARTESIAN_POINT('',(17.25,5.5,1.8));
#20054=CARTESIAN_POINT('',(20.5,4.5,1.8));
#20055=CARTESIAN_POINT('',(20.5,4.5,1.8));
#20056=CARTESIAN_POINT('',(22.,4.5,1.8));
#20057=CARTESIAN_POINT('',(22.,4.5,1.8));
#20058=CARTESIAN_POINT('',(22.,8.5,1.8));
#20059=CARTESIAN_POINT('',(22.,4.5,1.8));
#20060=CARTESIAN_POINT('',(14.,8.5,1.8));
#20061=CARTESIAN_POINT('',(22.,8.5,1.8));
#20062=CARTESIAN_POINT('',(14.,4.5,1.8));
#20063=CARTESIAN_POINT('',(14.,4.5,1.8));
#20064=CARTESIAN_POINT('',(22.,4.5,1.8));
#20065=CARTESIAN_POINT('Origin',(14.,4.5,1.));
#20066=CARTESIAN_POINT('',(14.,4.5,1.));
#20067=CARTESIAN_POINT('',(14.,4.5,1.8));
#20068=CARTESIAN_POINT('',(14.,8.5,1.));
#20069=CARTESIAN_POINT('',(14.,8.5,1.8));
#20070=CARTESIAN_POINT('',(14.,4.5,1.));
#20071=CARTESIAN_POINT('Origin',(22.,4.5,1.8));
#20072=CARTESIAN_POINT('',(22.,4.5,1.));
#20073=CARTESIAN_POINT('',(22.,4.5,1.));
#20074=CARTESIAN_POINT('',(22.,8.5,1.));
#20075=CARTESIAN_POINT('',(22.,4.5,1.));
#20076=CARTESIAN_POINT('',(22.,8.5,1.));
#20077=CARTESIAN_POINT('Origin',(18.,8.5,1.4));
#20078=CARTESIAN_POINT('',(14.,8.5,1.));
#20079=CARTESIAN_POINT('Origin',(15.5,4.5,1.));
#20080=CARTESIAN_POINT('',(20.5,4.5,18.));
#20081=CARTESIAN_POINT('',(20.5,4.5,1.));
#20082=CARTESIAN_POINT('',(15.5,4.5,18.));
#20083=CARTESIAN_POINT('',(15.5,4.5,18.));
#20084=CARTESIAN_POINT('',(15.5,4.5,1.));
#20085=CARTESIAN_POINT('',(14.,4.5,1.));
#20086=CARTESIAN_POINT('Origin',(20.5,4.5,1.));
#20087=CARTESIAN_POINT('',(20.5,5.5,18.));
#20088=CARTESIAN_POINT('',(20.5,5.5,1.));
#20089=CARTESIAN_POINT('',(20.5,4.5,18.));
#20090=CARTESIAN_POINT('Origin',(20.5,5.5,1.));
#20091=CARTESIAN_POINT('',(15.5,5.5,18.));
#20092=CARTESIAN_POINT('',(15.5,5.5,1.));
#20093=CARTESIAN_POINT('',(20.5,5.5,18.));
#20094=CARTESIAN_POINT('Origin',(15.5,5.5,1.));
#20095=CARTESIAN_POINT('',(15.5,5.5,18.));
#20096=CARTESIAN_POINT('Origin',(18.,5.,18.));
#20097=CARTESIAN_POINT('Origin',(18.,5.,1.));
#20098=CARTESIAN_POINT('',(0.,0.,0.));
#20099=CARTESIAN_POINT('Origin',(0.,-1.1,15.));
#20100=CARTESIAN_POINT('',(-0.165,-1.,15.));
#20101=CARTESIAN_POINT('Origin',(0.,-1.,15.));
#20102=CARTESIAN_POINT('',(-0.165,0.6,15.));
#20103=CARTESIAN_POINT('',(-0.165,-1.1,15.));
#20104=CARTESIAN_POINT('Origin',(0.,0.6,15.));
#20105=CARTESIAN_POINT('Origin',(0.,0.6,15.));
#20106=CARTESIAN_POINT('Origin',(1.15,4.,15.));
#20107=CARTESIAN_POINT('',(0.925,4.1,15.));
#20108=CARTESIAN_POINT('Origin',(1.15,4.1,15.));
#20109=CARTESIAN_POINT('',(0.925,4.5,15.));
#20110=CARTESIAN_POINT('',(0.925,4.,15.));
#20111=CARTESIAN_POINT('Origin',(1.15,4.5,15.));
#20112=CARTESIAN_POINT('Origin',(-0.575,4.,15.9959292143521));
#20113=CARTESIAN_POINT('',(-0.8,4.1,15.9959292143521));
#20114=CARTESIAN_POINT('Origin',(-0.575,4.1,15.9959292143521));
#20115=CARTESIAN_POINT('',(-0.8,4.5,15.9959292143521));
#20116=CARTESIAN_POINT('',(-0.8,4.,15.9959292143521));
#20117=CARTESIAN_POINT('Origin',(-0.575,4.5,15.9959292143521));
#20118=CARTESIAN_POINT('Origin',(-0.575000000000001,4.,14.0040707856479));
#20119=CARTESIAN_POINT('',(-0.8,4.1,14.0040707856479));
#20120=CARTESIAN_POINT('Origin',(-0.575000000000001,4.1,14.0040707856479));
#20121=CARTESIAN_POINT('',(-0.8,4.5,14.0040707856479));
#20122=CARTESIAN_POINT('',(-0.8,4.,14.0040707856479));
#20123=CARTESIAN_POINT('Origin',(-0.575000000000001,4.5,14.0040707856479));
#20124=CARTESIAN_POINT('Origin',(0.,4.5,15.));
#20125=CARTESIAN_POINT('',(-1.5,4.5,15.));
#20126=CARTESIAN_POINT('Origin',(0.,4.5,15.));
#20127=CARTESIAN_POINT('',(-0.6,4.5,15.));
#20128=CARTESIAN_POINT('Origin',(0.,4.5,15.));
#20129=CARTESIAN_POINT('Origin',(0.,4.1,15.));
#20130=CARTESIAN_POINT('',(-1.5,4.1,15.));
#20131=CARTESIAN_POINT('Origin',(0.,4.1,15.));
#20132=CARTESIAN_POINT('',(-0.6,4.1,15.));
#20133=CARTESIAN_POINT('Origin',(0.,4.1,15.));
#20134=CARTESIAN_POINT('Origin',(0.,4.1,15.));
#20135=CARTESIAN_POINT('',(-1.5,4.1,15.));
#20136=CARTESIAN_POINT('Origin',(0.,-1.,15.));
#20137=CARTESIAN_POINT('',(-0.6,-1.,15.));
#20138=CARTESIAN_POINT('',(-0.6,-1.,15.));
#20139=CARTESIAN_POINT('Origin',(0.,-1.,15.));
#20140=CARTESIAN_POINT('Origin',(0.,-1.,15.));
#20141=CARTESIAN_POINT('',(-0.6,5.5,15.));
#20142=CARTESIAN_POINT('Origin',(0.,5.5,15.));
#20143=CARTESIAN_POINT('',(-0.6,-1.,15.));
#20144=CARTESIAN_POINT('Origin',(0.,5.5,15.));
#20145=CARTESIAN_POINT('Origin',(0.,-1.,15.));
#20146=CARTESIAN_POINT('',(0.,0.,0.));
#20147=CARTESIAN_POINT('Origin',(0.,0.5,15.));
#20148=CARTESIAN_POINT('',(-0.605,4.1,15.));
#20149=CARTESIAN_POINT('Origin',(0.,4.1,15.));
#20150=CARTESIAN_POINT('',(-0.605,0.5,15.));
#20151=CARTESIAN_POINT('',(-0.605,0.5,15.));
#20152=CARTESIAN_POINT('Origin',(0.,0.5,15.));
#20153=CARTESIAN_POINT('Origin',(0.,0.5,15.));
#20154=CARTESIAN_POINT('',(-0.8,4.1,15.));
#20155=CARTESIAN_POINT('Origin',(0.,4.1,15.));
#20156=CARTESIAN_POINT('',(-0.8,0.5,15.));
#20157=CARTESIAN_POINT('',(-0.8,0.5,15.));
#20158=CARTESIAN_POINT('Origin',(0.,0.5,15.));
#20159=CARTESIAN_POINT('Origin',(0.,4.1,15.));
#20160=CARTESIAN_POINT('Origin',(0.,0.5,15.));
#20161=CARTESIAN_POINT('',(0.,0.,0.));
#20162=CARTESIAN_POINT('Origin',(0.,-1.,15.));
#20163=CARTESIAN_POINT('',(-0.605,-0.5,15.));
#20164=CARTESIAN_POINT('Origin',(0.,-0.5,15.));
#20165=CARTESIAN_POINT('',(-0.605,-1.,15.));
#20166=CARTESIAN_POINT('',(-0.605,-1.,15.));
#20167=CARTESIAN_POINT('Origin',(0.,-1.,15.));
#20168=CARTESIAN_POINT('Origin',(0.,-1.,15.));
#20169=CARTESIAN_POINT('',(-0.8,-0.5,15.));
#20170=CARTESIAN_POINT('Origin',(0.,-0.5,15.));
#20171=CARTESIAN_POINT('',(-0.8,-1.,15.));
#20172=CARTESIAN_POINT('',(-0.8,-1.,15.));
#20173=CARTESIAN_POINT('Origin',(0.,-1.,15.));
#20174=CARTESIAN_POINT('Origin',(0.,-0.5,15.));
#20175=CARTESIAN_POINT('Origin',(0.,-1.,15.));
#20176=CARTESIAN_POINT('',(0.,0.,0.));
#20177=CARTESIAN_POINT('Origin',(0.,-1.2,15.));
#20178=CARTESIAN_POINT('',(-0.225,-1.,15.));
#20179=CARTESIAN_POINT('Origin',(0.,-1.,15.));
#20180=CARTESIAN_POINT('',(-0.225,-1.2,15.));
#20181=CARTESIAN_POINT('',(-0.225,-1.2,15.));
#20182=CARTESIAN_POINT('Origin',(0.,-1.2,15.));
#20183=CARTESIAN_POINT('Origin',(0.,-1.2,15.));
#20184=CARTESIAN_POINT('',(-1.,-1.,15.));
#20185=CARTESIAN_POINT('Origin',(0.,-1.,15.));
#20186=CARTESIAN_POINT('',(-1.,-1.2,15.));
#20187=CARTESIAN_POINT('',(-1.,-1.2,15.));
#20188=CARTESIAN_POINT('Origin',(0.,-1.2,15.));
#20189=CARTESIAN_POINT('Origin',(0.,-1.,15.));
#20190=CARTESIAN_POINT('Origin',(0.,-1.2,15.));
#20191=CARTESIAN_POINT('',(0.,0.,0.));
#20192=CARTESIAN_POINT('Origin',(18.,-1.1,15.));
#20193=CARTESIAN_POINT('',(17.835,-1.,15.));
#20194=CARTESIAN_POINT('Origin',(18.,-1.,15.));
#20195=CARTESIAN_POINT('',(17.835,0.6,15.));
#20196=CARTESIAN_POINT('',(17.835,-1.1,15.));
#20197=CARTESIAN_POINT('Origin',(18.,0.6,15.));
#20198=CARTESIAN_POINT('Origin',(18.,0.6,15.));
#20199=CARTESIAN_POINT('Origin',(19.15,4.,15.));
#20200=CARTESIAN_POINT('',(18.925,4.1,15.));
#20201=CARTESIAN_POINT('Origin',(19.15,4.1,15.));
#20202=CARTESIAN_POINT('',(18.925,4.5,15.));
#20203=CARTESIAN_POINT('',(18.925,4.,15.));
#20204=CARTESIAN_POINT('Origin',(19.15,4.5,15.));
#20205=CARTESIAN_POINT('Origin',(17.425,4.,15.9959292143521));
#20206=CARTESIAN_POINT('',(17.2,4.1,15.9959292143521));
#20207=CARTESIAN_POINT('Origin',(17.425,4.1,15.9959292143521));
#20208=CARTESIAN_POINT('',(17.2,4.5,15.9959292143521));
#20209=CARTESIAN_POINT('',(17.2,4.,15.9959292143521));
#20210=CARTESIAN_POINT('Origin',(17.425,4.5,15.9959292143521));
#20211=CARTESIAN_POINT('Origin',(17.425,4.,14.0040707856479));
#20212=CARTESIAN_POINT('',(17.2,4.1,14.0040707856479));
#20213=CARTESIAN_POINT('Origin',(17.425,4.1,14.0040707856479));
#20214=CARTESIAN_POINT('',(17.2,4.5,14.0040707856479));
#20215=CARTESIAN_POINT('',(17.2,4.,14.0040707856479));
#20216=CARTESIAN_POINT('Origin',(17.425,4.5,14.0040707856479));
#20217=CARTESIAN_POINT('Origin',(18.,4.5,15.));
#20218=CARTESIAN_POINT('',(16.5,4.5,15.));
#20219=CARTESIAN_POINT('Origin',(18.,4.5,15.));
#20220=CARTESIAN_POINT('',(17.4,4.5,15.));
#20221=CARTESIAN_POINT('Origin',(18.,4.5,15.));
#20222=CARTESIAN_POINT('Origin',(18.,4.1,15.));
#20223=CARTESIAN_POINT('',(16.5,4.1,15.));
#20224=CARTESIAN_POINT('Origin',(18.,4.1,15.));
#20225=CARTESIAN_POINT('',(17.4,4.1,15.));
#20226=CARTESIAN_POINT('Origin',(18.,4.1,15.));
#20227=CARTESIAN_POINT('Origin',(18.,4.1,15.));
#20228=CARTESIAN_POINT('',(16.5,4.1,15.));
#20229=CARTESIAN_POINT('Origin',(18.,-1.,15.));
#20230=CARTESIAN_POINT('',(17.4,-1.,15.));
#20231=CARTESIAN_POINT('',(17.4,-1.,15.));
#20232=CARTESIAN_POINT('Origin',(18.,-1.,15.));
#20233=CARTESIAN_POINT('Origin',(18.,-1.,15.));
#20234=CARTESIAN_POINT('',(17.4,5.5,15.));
#20235=CARTESIAN_POINT('Origin',(18.,5.5,15.));
#20236=CARTESIAN_POINT('',(17.4,-1.,15.));
#20237=CARTESIAN_POINT('Origin',(18.,5.5,15.));
#20238=CARTESIAN_POINT('Origin',(18.,-1.,15.));
#20239=CARTESIAN_POINT('',(0.,0.,0.));
#20240=CARTESIAN_POINT('Origin',(18.,0.5,15.));
#20241=CARTESIAN_POINT('',(17.395,4.1,15.));
#20242=CARTESIAN_POINT('Origin',(18.,4.1,15.));
#20243=CARTESIAN_POINT('',(17.395,0.5,15.));
#20244=CARTESIAN_POINT('',(17.395,0.5,15.));
#20245=CARTESIAN_POINT('Origin',(18.,0.5,15.));
#20246=CARTESIAN_POINT('Origin',(18.,0.5,15.));
#20247=CARTESIAN_POINT('',(17.2,4.1,15.));
#20248=CARTESIAN_POINT('Origin',(18.,4.1,15.));
#20249=CARTESIAN_POINT('',(17.2,0.5,15.));
#20250=CARTESIAN_POINT('',(17.2,0.5,15.));
#20251=CARTESIAN_POINT('Origin',(18.,0.5,15.));
#20252=CARTESIAN_POINT('Origin',(18.,4.1,15.));
#20253=CARTESIAN_POINT('Origin',(18.,0.5,15.));
#20254=CARTESIAN_POINT('',(0.,0.,0.));
#20255=CARTESIAN_POINT('Origin',(18.,-1.,15.));
#20256=CARTESIAN_POINT('',(17.395,-0.5,15.));
#20257=CARTESIAN_POINT('Origin',(18.,-0.5,15.));
#20258=CARTESIAN_POINT('',(17.395,-1.,15.));
#20259=CARTESIAN_POINT('',(17.395,-1.,15.));
#20260=CARTESIAN_POINT('Origin',(18.,-1.,15.));
#20261=CARTESIAN_POINT('Origin',(18.,-1.,15.));
#20262=CARTESIAN_POINT('',(17.2,-0.5,15.));
#20263=CARTESIAN_POINT('Origin',(18.,-0.5,15.));
#20264=CARTESIAN_POINT('',(17.2,-1.,15.));
#20265=CARTESIAN_POINT('',(17.2,-1.,15.));
#20266=CARTESIAN_POINT('Origin',(18.,-1.,15.));
#20267=CARTESIAN_POINT('Origin',(18.,-0.5,15.));
#20268=CARTESIAN_POINT('Origin',(18.,-1.,15.));
#20269=CARTESIAN_POINT('',(0.,0.,0.));
#20270=CARTESIAN_POINT('Origin',(18.,-1.2,15.));
#20271=CARTESIAN_POINT('',(17.775,-1.,15.));
#20272=CARTESIAN_POINT('Origin',(18.,-1.,15.));
#20273=CARTESIAN_POINT('',(17.775,-1.2,15.));
#20274=CARTESIAN_POINT('',(17.775,-1.2,15.));
#20275=CARTESIAN_POINT('Origin',(18.,-1.2,15.));
#20276=CARTESIAN_POINT('Origin',(18.,-1.2,15.));
#20277=CARTESIAN_POINT('',(17.,-1.,15.));
#20278=CARTESIAN_POINT('Origin',(18.,-1.,15.));
#20279=CARTESIAN_POINT('',(17.,-1.2,15.));
#20280=CARTESIAN_POINT('',(17.,-1.2,15.));
#20281=CARTESIAN_POINT('Origin',(18.,-1.2,15.));
#20282=CARTESIAN_POINT('Origin',(18.,-1.,15.));
#20283=CARTESIAN_POINT('Origin',(18.,-1.2,15.));
#20284=CARTESIAN_POINT('',(0.,0.,0.));
#20285=CARTESIAN_POINT('Origin',(-10.1,-4.5,9.85));
#20286=CARTESIAN_POINT('',(-10.,-4.56873863542434,10.));
#20287=CARTESIAN_POINT('',(-10.,-4.43126136457566,10.));
#20288=CARTESIAN_POINT('Origin',(-10.,-4.5,9.85));
#20289=CARTESIAN_POINT('',(-9.,-4.56873863542434,10.));
#20290=CARTESIAN_POINT('',(-10.1,-4.56873863542434,10.));
#20291=CARTESIAN_POINT('',(-9.,-4.43126136457566,10.));
#20292=CARTESIAN_POINT('Origin',(-9.,-4.5,9.85));
#20293=CARTESIAN_POINT('',(-10.1,-4.43126136457566,10.));
#20294=CARTESIAN_POINT('Origin',(-10.1,-4.5,6.15));
#20295=CARTESIAN_POINT('',(-10.,-4.5,6.315));
#20296=CARTESIAN_POINT('Origin',(-10.,-4.5,6.15));
#20297=CARTESIAN_POINT('',(-9.,-4.5,6.315));
#20298=CARTESIAN_POINT('',(-10.1,-4.5,6.315));
#20299=CARTESIAN_POINT('Origin',(-9.,-4.5,6.15));
#20300=CARTESIAN_POINT('Origin',(-9.5,-4.5,10.));
#20301=CARTESIAN_POINT('',(-10.,-9.,10.));
#20302=CARTESIAN_POINT('',(-10.,0.,10.));
#20303=CARTESIAN_POINT('',(-9.,-9.,10.));
#20304=CARTESIAN_POINT('',(-10.,-9.,10.));
#20305=CARTESIAN_POINT('',(-9.,-9.,10.));
#20306=CARTESIAN_POINT('',(-9.9,-8.2,10.));
#20307=CARTESIAN_POINT('Origin',(-9.5,-8.2,10.));
#20308=CARTESIAN_POINT('Origin',(-9.,-9.,1.));
#20309=CARTESIAN_POINT('',(-9.,-9.,1.));
#20310=CARTESIAN_POINT('',(-9.,-9.,1.));
#20311=CARTESIAN_POINT('',(-9.,0.,1.));
#20312=CARTESIAN_POINT('',(-9.,-9.,1.));
#20313=CARTESIAN_POINT('',(-9.,0.,10.));
#20314=CARTESIAN_POINT('',(-9.,0.,1.));
#20315=CARTESIAN_POINT('',(-9.,-9.,10.));
#20316=CARTESIAN_POINT('',(-9.,-2.,8.605));
#20317=CARTESIAN_POINT('Origin',(-9.,-2.,8.));
#20318=CARTESIAN_POINT('',(-9.,-7.,8.605));
#20319=CARTESIAN_POINT('Origin',(-9.,-7.,8.));
#20320=CARTESIAN_POINT('',(-9.,-4.5,9.6));
#20321=CARTESIAN_POINT('Origin',(-9.,-4.5,8.));
#20322=CARTESIAN_POINT('Origin',(-9.5,-0.8,1.8));
#20323=CARTESIAN_POINT('',(-9.9,-0.8,1.8));
#20324=CARTESIAN_POINT('Origin',(-9.5,-0.8,1.8));
#20325=CARTESIAN_POINT('',(-9.9,-0.8,10.));
#20326=CARTESIAN_POINT('',(-9.9,-0.8,1.8));
#20327=CARTESIAN_POINT('Origin',(-9.5,-0.8,10.));
#20328=CARTESIAN_POINT('Origin',(-9.5,-0.8,1.8));
#20329=CARTESIAN_POINT('',(-9.725,-0.8,1.8));
#20330=CARTESIAN_POINT('Origin',(-9.5,-0.8,1.8));
#20331=CARTESIAN_POINT('Origin',(-9.5,-0.8,0.9));
#20332=CARTESIAN_POINT('',(-9.725,-0.8,1.));
#20333=CARTESIAN_POINT('Origin',(-9.5,-0.8,1.));
#20334=CARTESIAN_POINT('',(-9.725,-0.8,0.9));
#20335=CARTESIAN_POINT('Origin',(-9.5,-8.2,1.8));
#20336=CARTESIAN_POINT('',(-9.9,-8.2,1.8));
#20337=CARTESIAN_POINT('Origin',(-9.5,-8.2,1.8));
#20338=CARTESIAN_POINT('',(-9.9,-8.2,1.8));
#20339=CARTESIAN_POINT('Origin',(-9.5,-8.2,1.8));
#20340=CARTESIAN_POINT('',(-9.725,-8.2,1.8));
#20341=CARTESIAN_POINT('Origin',(-9.5,-8.2,1.8));
#20342=CARTESIAN_POINT('Origin',(-9.5,-8.2,0.9));
#20343=CARTESIAN_POINT('',(-9.725,-8.2,1.));
#20344=CARTESIAN_POINT('Origin',(-9.5,-8.2,1.));
#20345=CARTESIAN_POINT('',(-9.725,-8.2,0.9));
#20346=CARTESIAN_POINT('Origin',(-10.1,-4.5,8.));
#20347=CARTESIAN_POINT('',(-10.,-4.5,9.6));
#20348=CARTESIAN_POINT('Origin',(-10.,-4.5,8.));
#20349=CARTESIAN_POINT('',(-10.1,-4.5,9.6));
#20350=CARTESIAN_POINT('Origin',(-10.1,-7.,8.));
#20351=CARTESIAN_POINT('',(-10.,-7.,8.605));
#20352=CARTESIAN_POINT('Origin',(-10.,-7.,8.));
#20353=CARTESIAN_POINT('',(-10.1,-7.,8.605));
#20354=CARTESIAN_POINT('Origin',(-10.1,-2.,8.));
#20355=CARTESIAN_POINT('',(-10.,-2.,8.605));
#20356=CARTESIAN_POINT('Origin',(-10.,-2.,8.));
#20357=CARTESIAN_POINT('',(-10.1,-2.,8.605));
#20358=CARTESIAN_POINT('Origin',(-9.,0.,1.));
#20359=CARTESIAN_POINT('',(-10.,0.,1.));
#20360=CARTESIAN_POINT('',(-9.,0.,1.));
#20361=CARTESIAN_POINT('',(-10.,0.,10.));
#20362=CARTESIAN_POINT('',(-10.,0.,1.));
#20363=CARTESIAN_POINT('',(-9.,0.,10.));
#20364=CARTESIAN_POINT('Origin',(-10.,-9.,1.));
#20365=CARTESIAN_POINT('',(-10.,-9.,1.));
#20366=CARTESIAN_POINT('',(-10.,-9.,1.));
#20367=CARTESIAN_POINT('',(-10.,-9.,1.));
#20368=CARTESIAN_POINT('Origin',(-10.,0.,1.));
#20369=CARTESIAN_POINT('',(-10.,0.,10.));
#20370=CARTESIAN_POINT('',(-10.,0.,1.));
#20371=CARTESIAN_POINT('Origin',(-9.5,-4.5,10.));
#20372=CARTESIAN_POINT('Origin',(-9.5,-4.5,1.));
#20373=CARTESIAN_POINT('',(0.,0.,0.));
#20374=CARTESIAN_POINT('Origin',(-10.3,-4.5,9.85));
#20375=CARTESIAN_POINT('',(-10.2,-4.5,10.075));
#20376=CARTESIAN_POINT('Origin',(-10.2,-4.5,9.85));
#20377=CARTESIAN_POINT('',(-10.,-4.5,10.075));
#20378=CARTESIAN_POINT('',(-10.3,-4.5,10.075));
#20379=CARTESIAN_POINT('Origin',(-10.,-4.5,9.85));
#20380=CARTESIAN_POINT('Origin',(-10.3,-4.5,6.15));
#20381=CARTESIAN_POINT('',(-10.2,-4.5,6.375));
#20382=CARTESIAN_POINT('Origin',(-10.2,-4.5,6.15));
#20383=CARTESIAN_POINT('',(-10.,-4.5,6.375));
#20384=CARTESIAN_POINT('',(-10.3,-4.5,6.375));
#20385=CARTESIAN_POINT('Origin',(-10.,-4.5,6.15));
#20386=CARTESIAN_POINT('Origin',(-10.3,-7.,8.));
#20387=CARTESIAN_POINT('',(-10.,-6.55758,7.58004221212127));
#20388=CARTESIAN_POINT('',(-10.2,-6.55758,7.58004221212127));
#20389=CARTESIAN_POINT('',(-10.3,-6.55758,7.58004221212127));
#20390=CARTESIAN_POINT('',(-10.,-6.55758,8.41995778787873));
#20391=CARTESIAN_POINT('Origin',(-10.,-7.,8.));
#20392=CARTESIAN_POINT('',(-10.2,-6.55758,8.41995778787873));
#20393=CARTESIAN_POINT('',(-10.3,-6.55758,8.41995778787873));
#20394=CARTESIAN_POINT('Origin',(-10.2,-7.,8.));
#20395=CARTESIAN_POINT('Origin',(-10.3,-2.,8.));
#20396=CARTESIAN_POINT('',(-10.,-2.44242,8.41995778787873));
#20397=CARTESIAN_POINT('',(-10.2,-2.44242,8.41995778787873));
#20398=CARTESIAN_POINT('',(-10.3,-2.44242,8.41995778787873));
#20399=CARTESIAN_POINT('',(-10.,-2.44242,7.58004221212127));
#20400=CARTESIAN_POINT('Origin',(-10.,-2.,8.));
#20401=CARTESIAN_POINT('',(-10.2,-2.44242,7.58004221212127));
#20402=CARTESIAN_POINT('',(-10.3,-2.44242,7.58004221212127));
#20403=CARTESIAN_POINT('Origin',(-10.2,-2.,8.));
#20404=CARTESIAN_POINT('Origin',(-10.,-4.5,8.));
#20405=CARTESIAN_POINT('Origin',(-10.,-4.5,8.));
#20406=CARTESIAN_POINT('Origin',(-10.,-4.5,8.));
#20407=CARTESIAN_POINT('',(-10.,-4.5,9.02));
#20408=CARTESIAN_POINT('Origin',(-10.,-4.5,8.));
#20409=CARTESIAN_POINT('Origin',(-10.2,-4.5,8.));
#20410=CARTESIAN_POINT('Origin',(-10.2,-4.5,8.));
#20411=CARTESIAN_POINT('Origin',(-10.2,-4.5,8.));
#20412=CARTESIAN_POINT('Origin',(-10.2,-4.5,8.));
#20413=CARTESIAN_POINT('Origin',(-10.2,-4.5,8.));
#20414=CARTESIAN_POINT('',(-10.2,-4.5,9.02));
#20415=CARTESIAN_POINT('',(-10.2,-4.5,9.02));
#20416=CARTESIAN_POINT('Origin',(-10.2,-4.5,8.));
#20417=CARTESIAN_POINT('Origin',(-10.2,-4.5,8.));
#20418=CARTESIAN_POINT('',(0.,0.,0.));
#20419=CARTESIAN_POINT('Origin',(-10.2,-4.5,9.85));
#20420=CARTESIAN_POINT('',(-10.2,-4.5,10.2));
#20421=CARTESIAN_POINT('Origin',(-10.2,-4.5,9.85));
#20422=CARTESIAN_POINT('',(-10.2,-4.5,10.05));
#20423=CARTESIAN_POINT('Origin',(-10.2,-4.5,9.85));
#20424=CARTESIAN_POINT('Origin',(-10.6,-4.5,9.85));
#20425=CARTESIAN_POINT('',(-10.6,-4.5,10.2));
#20426=CARTESIAN_POINT('',(-10.6,-4.5,10.2));
#20427=CARTESIAN_POINT('Origin',(-10.6,-4.5,9.85));
#20428=CARTESIAN_POINT('Origin',(-10.6,-4.5,9.85));
#20429=CARTESIAN_POINT('Origin',(-10.2,-4.5,9.85));
#20430=CARTESIAN_POINT('',(-9.5,-4.5,10.05));
#20431=CARTESIAN_POINT('Origin',(-9.5,-4.5,9.85));
#20432=CARTESIAN_POINT('',(-10.2,-4.5,10.05));
#20433=CARTESIAN_POINT('Origin',(-9.5,-4.5,9.85));
#20434=CARTESIAN_POINT('',(0.,0.,0.));
#20435=CARTESIAN_POINT('Origin',(-10.2,-4.5,6.15));
#20436=CARTESIAN_POINT('',(-10.2,-4.5,6.5));
#20437=CARTESIAN_POINT('Origin',(-10.2,-4.5,6.15));
#20438=CARTESIAN_POINT('',(-10.2,-4.5,6.35));
#20439=CARTESIAN_POINT('Origin',(-10.2,-4.5,6.15));
#20440=CARTESIAN_POINT('Origin',(-10.6,-4.5,6.15));
#20441=CARTESIAN_POINT('',(-10.6,-4.5,6.5));
#20442=CARTESIAN_POINT('',(-10.6,-4.5,6.5));
#20443=CARTESIAN_POINT('Origin',(-10.6,-4.5,6.15));
#20444=CARTESIAN_POINT('Origin',(-10.6,-4.5,6.15));
#20445=CARTESIAN_POINT('Origin',(-10.2,-4.5,6.15));
#20446=CARTESIAN_POINT('',(-9.5,-4.5,6.35));
#20447=CARTESIAN_POINT('Origin',(-9.5,-4.5,6.15));
#20448=CARTESIAN_POINT('',(-10.2,-4.5,6.35));
#20449=CARTESIAN_POINT('Origin',(-9.5,-4.5,6.15));
#20450=CARTESIAN_POINT('',(0.,0.,0.));
#20451=CARTESIAN_POINT('Origin',(-9.1,-4.5,9.85));
#20452=CARTESIAN_POINT('',(-9.,-4.5,10.075));
#20453=CARTESIAN_POINT('Origin',(-9.,-4.5,9.85));
#20454=CARTESIAN_POINT('',(-8.8,-4.5,10.075));
#20455=CARTESIAN_POINT('',(-9.1,-4.5,10.075));
#20456=CARTESIAN_POINT('Origin',(-8.8,-4.5,9.85));
#20457=CARTESIAN_POINT('Origin',(-9.1,-4.5,6.15));
#20458=CARTESIAN_POINT('',(-9.,-4.5,6.375));
#20459=CARTESIAN_POINT('Origin',(-9.,-4.5,6.15));
#20460=CARTESIAN_POINT('',(-8.8,-4.5,6.375));
#20461=CARTESIAN_POINT('',(-9.1,-4.5,6.375));
#20462=CARTESIAN_POINT('Origin',(-8.8,-4.5,6.15));
#20463=CARTESIAN_POINT('Origin',(-9.1,-7.,8.));
#20464=CARTESIAN_POINT('',(-8.8,-6.55758,7.58004221212127));
#20465=CARTESIAN_POINT('',(-9.,-6.55758,7.58004221212127));
#20466=CARTESIAN_POINT('',(-9.1,-6.55758,7.58004221212127));
#20467=CARTESIAN_POINT('',(-8.8,-6.55758,8.41995778787873));
#20468=CARTESIAN_POINT('Origin',(-8.8,-7.,8.));
#20469=CARTESIAN_POINT('',(-9.,-6.55758,8.41995778787873));
#20470=CARTESIAN_POINT('',(-9.1,-6.55758,8.41995778787873));
#20471=CARTESIAN_POINT('Origin',(-9.,-7.,8.));
#20472=CARTESIAN_POINT('Origin',(-9.1,-2.,8.));
#20473=CARTESIAN_POINT('',(-8.8,-2.44242,8.41995778787873));
#20474=CARTESIAN_POINT('',(-9.,-2.44242,8.41995778787873));
#20475=CARTESIAN_POINT('',(-9.1,-2.44242,8.41995778787873));
#20476=CARTESIAN_POINT('',(-8.8,-2.44242,7.58004221212127));
#20477=CARTESIAN_POINT('Origin',(-8.8,-2.,8.));
#20478=CARTESIAN_POINT('',(-9.,-2.44242,7.58004221212127));
#20479=CARTESIAN_POINT('',(-9.1,-2.44242,7.58004221212127));
#20480=CARTESIAN_POINT('Origin',(-9.,-2.,8.));
#20481=CARTESIAN_POINT('Origin',(-8.8,-4.5,8.));
#20482=CARTESIAN_POINT('Origin',(-8.8,-4.5,8.));
#20483=CARTESIAN_POINT('Origin',(-8.8,-4.5,8.));
#20484=CARTESIAN_POINT('',(-8.8,-4.5,9.02));
#20485=CARTESIAN_POINT('Origin',(-8.8,-4.5,8.));
#20486=CARTESIAN_POINT('Origin',(-9.,-4.5,8.));
#20487=CARTESIAN_POINT('Origin',(-9.,-4.5,8.));
#20488=CARTESIAN_POINT('Origin',(-9.,-4.5,8.));
#20489=CARTESIAN_POINT('Origin',(-9.,-4.5,8.));
#20490=CARTESIAN_POINT('Origin',(-9.,-4.5,8.));
#20491=CARTESIAN_POINT('',(-9.,-4.5,9.02));
#20492=CARTESIAN_POINT('',(-9.,-4.5,9.02));
#20493=CARTESIAN_POINT('Origin',(-9.,-4.5,8.));
#20494=CARTESIAN_POINT('Origin',(-9.,-4.5,8.));
#20495=CARTESIAN_POINT('',(0.,0.,0.));
#20496=CARTESIAN_POINT('Origin',(-8.8,-4.5,9.85));
#20497=CARTESIAN_POINT('',(-8.8,-4.5,10.2));
#20498=CARTESIAN_POINT('Origin',(-8.8,-4.5,9.85));
#20499=CARTESIAN_POINT('',(-8.8,-4.5,10.05));
#20500=CARTESIAN_POINT('Origin',(-8.8,-4.5,9.85));
#20501=CARTESIAN_POINT('Origin',(-8.8,-4.5,9.85));
#20502=CARTESIAN_POINT('',(-8.4,-4.5,10.2));
#20503=CARTESIAN_POINT('Origin',(-8.4,-4.5,9.85));
#20504=CARTESIAN_POINT('',(-8.8,-4.5,10.2));
#20505=CARTESIAN_POINT('Origin',(-8.4,-4.5,9.85));
#20506=CARTESIAN_POINT('Origin',(-9.5,-4.5,9.85));
#20507=CARTESIAN_POINT('',(-9.5,-4.5,10.05));
#20508=CARTESIAN_POINT('',(-9.5,-4.5,10.05));
#20509=CARTESIAN_POINT('Origin',(-9.5,-4.5,9.85));
#20510=CARTESIAN_POINT('Origin',(-9.5,-4.5,9.85));
#20511=CARTESIAN_POINT('',(0.,0.,0.));
#20512=CARTESIAN_POINT('Origin',(-8.8,-4.5,6.15));
#20513=CARTESIAN_POINT('',(-8.8,-4.5,6.5));
#20514=CARTESIAN_POINT('Origin',(-8.8,-4.5,6.15));
#20515=CARTESIAN_POINT('',(-8.8,-4.5,6.35));
#20516=CARTESIAN_POINT('Origin',(-8.8,-4.5,6.15));
#20517=CARTESIAN_POINT('Origin',(-8.8,-4.5,6.15));
#20518=CARTESIAN_POINT('',(-8.4,-4.5,6.5));
#20519=CARTESIAN_POINT('Origin',(-8.4,-4.5,6.15));
#20520=CARTESIAN_POINT('',(-8.8,-4.5,6.5));
#20521=CARTESIAN_POINT('Origin',(-8.4,-4.5,6.15));
#20522=CARTESIAN_POINT('Origin',(-9.5,-4.5,6.15));
#20523=CARTESIAN_POINT('',(-9.5,-4.5,6.35));
#20524=CARTESIAN_POINT('',(-9.5,-4.5,6.35));
#20525=CARTESIAN_POINT('Origin',(-9.5,-4.5,6.15));
#20526=CARTESIAN_POINT('Origin',(-9.5,-4.5,6.15));
#20527=CARTESIAN_POINT('',(0.,0.,0.));
#20528=CARTESIAN_POINT('Origin',(-0.1,-4.5,9.85));
#20529=CARTESIAN_POINT('',(0.,-4.56873863542434,10.));
#20530=CARTESIAN_POINT('',(0.,-4.43126136457566,10.));
#20531=CARTESIAN_POINT('Origin',(0.,-4.5,9.85));
#20532=CARTESIAN_POINT('',(1.,-4.56873863542434,10.));
#20533=CARTESIAN_POINT('',(-0.1,-4.56873863542434,10.));
#20534=CARTESIAN_POINT('',(1.,-4.43126136457566,10.));
#20535=CARTESIAN_POINT('Origin',(1.,-4.5,9.85));
#20536=CARTESIAN_POINT('',(-0.1,-4.43126136457566,10.));
#20537=CARTESIAN_POINT('Origin',(-0.1,-4.5,6.15));
#20538=CARTESIAN_POINT('',(0.,-4.5,6.315));
#20539=CARTESIAN_POINT('Origin',(0.,-4.5,6.15));
#20540=CARTESIAN_POINT('',(1.,-4.5,6.315));
#20541=CARTESIAN_POINT('',(-0.1,-4.5,6.315));
#20542=CARTESIAN_POINT('Origin',(1.,-4.5,6.15));
#20543=CARTESIAN_POINT('Origin',(0.5,-4.5,10.));
#20544=CARTESIAN_POINT('',(0.,-9.,10.));
#20545=CARTESIAN_POINT('',(0.,0.,10.));
#20546=CARTESIAN_POINT('',(1.,-9.,10.));
#20547=CARTESIAN_POINT('',(0.,-9.,10.));
#20548=CARTESIAN_POINT('',(1.,-9.,10.));
#20549=CARTESIAN_POINT('',(0.1,-8.2,10.));
#20550=CARTESIAN_POINT('Origin',(0.5,-8.2,10.));
#20551=CARTESIAN_POINT('Origin',(1.,-9.,1.));
#20552=CARTESIAN_POINT('',(1.,-9.,1.));
#20553=CARTESIAN_POINT('',(1.,-9.,1.));
#20554=CARTESIAN_POINT('',(1.,0.,1.));
#20555=CARTESIAN_POINT('',(1.,-9.,1.));
#20556=CARTESIAN_POINT('',(1.,0.,10.));
#20557=CARTESIAN_POINT('',(1.,0.,1.));
#20558=CARTESIAN_POINT('',(1.,-9.,10.));
#20559=CARTESIAN_POINT('',(1.,-2.,8.605));
#20560=CARTESIAN_POINT('Origin',(1.,-2.,8.));
#20561=CARTESIAN_POINT('',(1.,-7.,8.605));
#20562=CARTESIAN_POINT('Origin',(1.,-7.,8.));
#20563=CARTESIAN_POINT('',(1.,-4.5,9.6));
#20564=CARTESIAN_POINT('Origin',(1.,-4.5,8.));
#20565=CARTESIAN_POINT('Origin',(0.5,-0.8,1.8));
#20566=CARTESIAN_POINT('',(0.1,-0.8,1.8));
#20567=CARTESIAN_POINT('Origin',(0.5,-0.8,1.8));
#20568=CARTESIAN_POINT('',(0.1,-0.8,10.));
#20569=CARTESIAN_POINT('',(0.1,-0.8,1.8));
#20570=CARTESIAN_POINT('Origin',(0.5,-0.8,10.));
#20571=CARTESIAN_POINT('Origin',(0.5,-0.8,1.8));
#20572=CARTESIAN_POINT('',(0.275,-0.8,1.8));
#20573=CARTESIAN_POINT('Origin',(0.5,-0.8,1.8));
#20574=CARTESIAN_POINT('Origin',(0.5,-0.8,0.9));
#20575=CARTESIAN_POINT('',(0.275,-0.8,1.));
#20576=CARTESIAN_POINT('Origin',(0.5,-0.8,1.));
#20577=CARTESIAN_POINT('',(0.275,-0.8,0.9));
#20578=CARTESIAN_POINT('Origin',(0.5,-8.2,1.8));
#20579=CARTESIAN_POINT('',(0.1,-8.2,1.8));
#20580=CARTESIAN_POINT('Origin',(0.5,-8.2,1.8));
#20581=CARTESIAN_POINT('',(0.1,-8.2,1.8));
#20582=CARTESIAN_POINT('Origin',(0.5,-8.2,1.8));
#20583=CARTESIAN_POINT('',(0.275,-8.2,1.8));
#20584=CARTESIAN_POINT('Origin',(0.5,-8.2,1.8));
#20585=CARTESIAN_POINT('Origin',(0.5,-8.2,0.9));
#20586=CARTESIAN_POINT('',(0.275,-8.2,1.));
#20587=CARTESIAN_POINT('Origin',(0.5,-8.2,1.));
#20588=CARTESIAN_POINT('',(0.275,-8.2,0.9));
#20589=CARTESIAN_POINT('Origin',(-0.1,-4.5,8.));
#20590=CARTESIAN_POINT('',(0.,-4.5,9.6));
#20591=CARTESIAN_POINT('Origin',(0.,-4.5,8.));
#20592=CARTESIAN_POINT('',(-0.1,-4.5,9.6));
#20593=CARTESIAN_POINT('Origin',(-0.1,-7.,8.));
#20594=CARTESIAN_POINT('',(0.,-7.,8.605));
#20595=CARTESIAN_POINT('Origin',(0.,-7.,8.));
#20596=CARTESIAN_POINT('',(-0.1,-7.,8.605));
#20597=CARTESIAN_POINT('Origin',(-0.1,-2.,8.));
#20598=CARTESIAN_POINT('',(0.,-2.,8.605));
#20599=CARTESIAN_POINT('Origin',(0.,-2.,8.));
#20600=CARTESIAN_POINT('',(-0.1,-2.,8.605));
#20601=CARTESIAN_POINT('Origin',(1.,0.,1.));
#20602=CARTESIAN_POINT('',(0.,0.,1.));
#20603=CARTESIAN_POINT('',(1.,0.,1.));
#20604=CARTESIAN_POINT('',(0.,0.,10.));
#20605=CARTESIAN_POINT('',(0.,0.,1.));
#20606=CARTESIAN_POINT('',(1.,0.,10.));
#20607=CARTESIAN_POINT('Origin',(0.,-9.,1.));
#20608=CARTESIAN_POINT('',(0.,-9.,1.));
#20609=CARTESIAN_POINT('',(0.,-9.,1.));
#20610=CARTESIAN_POINT('',(0.,-9.,1.));
#20611=CARTESIAN_POINT('Origin',(0.,0.,1.));
#20612=CARTESIAN_POINT('',(0.,0.,10.));
#20613=CARTESIAN_POINT('',(0.,0.,1.));
#20614=CARTESIAN_POINT('Origin',(0.5,-4.5,10.));
#20615=CARTESIAN_POINT('Origin',(0.5,-4.5,1.));
#20616=CARTESIAN_POINT('',(0.,0.,0.));
#20617=CARTESIAN_POINT('Origin',(-0.3,-4.5,9.85));
#20618=CARTESIAN_POINT('',(-0.2,-4.5,10.075));
#20619=CARTESIAN_POINT('Origin',(-0.2,-4.5,9.85));
#20620=CARTESIAN_POINT('',(0.,-4.5,10.075));
#20621=CARTESIAN_POINT('',(-0.3,-4.5,10.075));
#20622=CARTESIAN_POINT('Origin',(0.,-4.5,9.85));
#20623=CARTESIAN_POINT('Origin',(-0.3,-4.5,6.15));
#20624=CARTESIAN_POINT('',(-0.2,-4.5,6.375));
#20625=CARTESIAN_POINT('Origin',(-0.2,-4.5,6.15));
#20626=CARTESIAN_POINT('',(0.,-4.5,6.375));
#20627=CARTESIAN_POINT('',(-0.3,-4.5,6.375));
#20628=CARTESIAN_POINT('Origin',(0.,-4.5,6.15));
#20629=CARTESIAN_POINT('Origin',(-0.3,-7.,8.));
#20630=CARTESIAN_POINT('',(0.,-6.55758,7.58004221212127));
#20631=CARTESIAN_POINT('',(-0.2,-6.55758,7.58004221212127));
#20632=CARTESIAN_POINT('',(-0.3,-6.55758,7.58004221212127));
#20633=CARTESIAN_POINT('',(0.,-6.55758,8.41995778787873));
#20634=CARTESIAN_POINT('Origin',(0.,-7.,8.));
#20635=CARTESIAN_POINT('',(-0.2,-6.55758,8.41995778787873));
#20636=CARTESIAN_POINT('',(-0.3,-6.55758,8.41995778787873));
#20637=CARTESIAN_POINT('Origin',(-0.2,-7.,8.));
#20638=CARTESIAN_POINT('Origin',(-0.3,-2.,8.));
#20639=CARTESIAN_POINT('',(0.,-2.44242,8.41995778787873));
#20640=CARTESIAN_POINT('',(-0.2,-2.44242,8.41995778787873));
#20641=CARTESIAN_POINT('',(-0.3,-2.44242,8.41995778787873));
#20642=CARTESIAN_POINT('',(0.,-2.44242,7.58004221212127));
#20643=CARTESIAN_POINT('Origin',(0.,-2.,8.));
#20644=CARTESIAN_POINT('',(-0.2,-2.44242,7.58004221212127));
#20645=CARTESIAN_POINT('',(-0.3,-2.44242,7.58004221212127));
#20646=CARTESIAN_POINT('Origin',(-0.2,-2.,8.));
#20647=CARTESIAN_POINT('Origin',(0.,-4.5,8.));
#20648=CARTESIAN_POINT('Origin',(0.,-4.5,8.));
#20649=CARTESIAN_POINT('Origin',(0.,-4.5,8.));
#20650=CARTESIAN_POINT('',(0.,-4.5,9.02));
#20651=CARTESIAN_POINT('Origin',(0.,-4.5,8.));
#20652=CARTESIAN_POINT('Origin',(-0.2,-4.5,8.));
#20653=CARTESIAN_POINT('Origin',(-0.2,-4.5,8.));
#20654=CARTESIAN_POINT('Origin',(-0.2,-4.5,8.));
#20655=CARTESIAN_POINT('Origin',(-0.2,-4.5,8.));
#20656=CARTESIAN_POINT('Origin',(-0.2,-4.5,8.));
#20657=CARTESIAN_POINT('',(-0.2,-4.5,9.02));
#20658=CARTESIAN_POINT('',(-0.2,-4.5,9.02));
#20659=CARTESIAN_POINT('Origin',(-0.2,-4.5,8.));
#20660=CARTESIAN_POINT('Origin',(-0.2,-4.5,8.));
#20661=CARTESIAN_POINT('',(0.,0.,0.));
#20662=CARTESIAN_POINT('Origin',(-0.2,-4.5,9.85));
#20663=CARTESIAN_POINT('',(-0.2,-4.5,10.2));
#20664=CARTESIAN_POINT('Origin',(-0.2,-4.5,9.85));
#20665=CARTESIAN_POINT('',(-0.2,-4.5,10.05));
#20666=CARTESIAN_POINT('Origin',(-0.2,-4.5,9.85));
#20667=CARTESIAN_POINT('Origin',(-0.6,-4.5,9.85));
#20668=CARTESIAN_POINT('',(-0.6,-4.5,10.2));
#20669=CARTESIAN_POINT('',(-0.6,-4.5,10.2));
#20670=CARTESIAN_POINT('Origin',(-0.6,-4.5,9.85));
#20671=CARTESIAN_POINT('Origin',(-0.6,-4.5,9.85));
#20672=CARTESIAN_POINT('Origin',(-0.2,-4.5,9.85));
#20673=CARTESIAN_POINT('',(0.5,-4.5,10.05));
#20674=CARTESIAN_POINT('Origin',(0.5,-4.5,9.85));
#20675=CARTESIAN_POINT('',(-0.2,-4.5,10.05));
#20676=CARTESIAN_POINT('Origin',(0.5,-4.5,9.85));
#20677=CARTESIAN_POINT('',(0.,0.,0.));
#20678=CARTESIAN_POINT('Origin',(-0.2,-4.5,6.15));
#20679=CARTESIAN_POINT('',(-0.2,-4.5,6.5));
#20680=CARTESIAN_POINT('Origin',(-0.2,-4.5,6.15));
#20681=CARTESIAN_POINT('',(-0.2,-4.5,6.35));
#20682=CARTESIAN_POINT('Origin',(-0.2,-4.5,6.15));
#20683=CARTESIAN_POINT('Origin',(-0.6,-4.5,6.15));
#20684=CARTESIAN_POINT('',(-0.6,-4.5,6.5));
#20685=CARTESIAN_POINT('',(-0.6,-4.5,6.5));
#20686=CARTESIAN_POINT('Origin',(-0.6,-4.5,6.15));
#20687=CARTESIAN_POINT('Origin',(-0.6,-4.5,6.15));
#20688=CARTESIAN_POINT('Origin',(-0.2,-4.5,6.15));
#20689=CARTESIAN_POINT('',(0.5,-4.5,6.35));
#20690=CARTESIAN_POINT('Origin',(0.5,-4.5,6.15));
#20691=CARTESIAN_POINT('',(-0.2,-4.5,6.35));
#20692=CARTESIAN_POINT('Origin',(0.5,-4.5,6.15));
#20693=CARTESIAN_POINT('',(0.,0.,0.));
#20694=CARTESIAN_POINT('Origin',(0.9,-4.5,9.85));
#20695=CARTESIAN_POINT('',(1.,-4.5,10.075));
#20696=CARTESIAN_POINT('Origin',(1.,-4.5,9.85));
#20697=CARTESIAN_POINT('',(1.2,-4.5,10.075));
#20698=CARTESIAN_POINT('',(0.9,-4.5,10.075));
#20699=CARTESIAN_POINT('Origin',(1.2,-4.5,9.85));
#20700=CARTESIAN_POINT('Origin',(0.9,-4.5,6.15));
#20701=CARTESIAN_POINT('',(1.,-4.5,6.375));
#20702=CARTESIAN_POINT('Origin',(1.,-4.5,6.15));
#20703=CARTESIAN_POINT('',(1.2,-4.5,6.375));
#20704=CARTESIAN_POINT('',(0.9,-4.5,6.375));
#20705=CARTESIAN_POINT('Origin',(1.2,-4.5,6.15));
#20706=CARTESIAN_POINT('Origin',(0.9,-7.,8.));
#20707=CARTESIAN_POINT('',(1.2,-6.55758,7.58004221212127));
#20708=CARTESIAN_POINT('',(1.,-6.55758,7.58004221212127));
#20709=CARTESIAN_POINT('',(0.9,-6.55758,7.58004221212127));
#20710=CARTESIAN_POINT('',(1.2,-6.55758,8.41995778787873));
#20711=CARTESIAN_POINT('Origin',(1.2,-7.,8.));
#20712=CARTESIAN_POINT('',(1.,-6.55758,8.41995778787873));
#20713=CARTESIAN_POINT('',(0.9,-6.55758,8.41995778787873));
#20714=CARTESIAN_POINT('Origin',(1.,-7.,8.));
#20715=CARTESIAN_POINT('Origin',(0.9,-2.,8.));
#20716=CARTESIAN_POINT('',(1.2,-2.44242,8.41995778787873));
#20717=CARTESIAN_POINT('',(1.,-2.44242,8.41995778787873));
#20718=CARTESIAN_POINT('',(0.9,-2.44242,8.41995778787873));
#20719=CARTESIAN_POINT('',(1.2,-2.44242,7.58004221212127));
#20720=CARTESIAN_POINT('Origin',(1.2,-2.,8.));
#20721=CARTESIAN_POINT('',(1.,-2.44242,7.58004221212127));
#20722=CARTESIAN_POINT('',(0.9,-2.44242,7.58004221212127));
#20723=CARTESIAN_POINT('Origin',(1.,-2.,8.));
#20724=CARTESIAN_POINT('Origin',(1.2,-4.5,8.));
#20725=CARTESIAN_POINT('Origin',(1.2,-4.5,8.));
#20726=CARTESIAN_POINT('Origin',(1.2,-4.5,8.));
#20727=CARTESIAN_POINT('',(1.2,-4.5,9.02));
#20728=CARTESIAN_POINT('Origin',(1.2,-4.5,8.));
#20729=CARTESIAN_POINT('Origin',(1.,-4.5,8.));
#20730=CARTESIAN_POINT('Origin',(1.,-4.5,8.));
#20731=CARTESIAN_POINT('Origin',(1.,-4.5,8.));
#20732=CARTESIAN_POINT('Origin',(1.,-4.5,8.));
#20733=CARTESIAN_POINT('Origin',(1.,-4.5,8.));
#20734=CARTESIAN_POINT('',(1.,-4.5,9.02));
#20735=CARTESIAN_POINT('',(1.,-4.5,9.02));
#20736=CARTESIAN_POINT('Origin',(1.,-4.5,8.));
#20737=CARTESIAN_POINT('Origin',(1.,-4.5,8.));
#20738=CARTESIAN_POINT('',(0.,0.,0.));
#20739=CARTESIAN_POINT('Origin',(1.2,-4.5,9.85));
#20740=CARTESIAN_POINT('',(1.2,-4.5,10.2));
#20741=CARTESIAN_POINT('Origin',(1.2,-4.5,9.85));
#20742=CARTESIAN_POINT('',(1.2,-4.5,10.05));
#20743=CARTESIAN_POINT('Origin',(1.2,-4.5,9.85));
#20744=CARTESIAN_POINT('Origin',(1.2,-4.5,9.85));
#20745=CARTESIAN_POINT('',(1.6,-4.5,10.2));
#20746=CARTESIAN_POINT('Origin',(1.6,-4.5,9.85));
#20747=CARTESIAN_POINT('',(1.2,-4.5,10.2));
#20748=CARTESIAN_POINT('Origin',(1.6,-4.5,9.85));
#20749=CARTESIAN_POINT('Origin',(0.5,-4.5,9.85));
#20750=CARTESIAN_POINT('',(0.5,-4.5,10.05));
#20751=CARTESIAN_POINT('',(0.5,-4.5,10.05));
#20752=CARTESIAN_POINT('Origin',(0.5,-4.5,9.85));
#20753=CARTESIAN_POINT('Origin',(0.5,-4.5,9.85));
#20754=CARTESIAN_POINT('',(0.,0.,0.));
#20755=CARTESIAN_POINT('Origin',(1.2,-4.5,6.15));
#20756=CARTESIAN_POINT('',(1.2,-4.5,6.5));
#20757=CARTESIAN_POINT('Origin',(1.2,-4.5,6.15));
#20758=CARTESIAN_POINT('',(1.2,-4.5,6.35));
#20759=CARTESIAN_POINT('Origin',(1.2,-4.5,6.15));
#20760=CARTESIAN_POINT('Origin',(1.2,-4.5,6.15));
#20761=CARTESIAN_POINT('',(1.6,-4.5,6.5));
#20762=CARTESIAN_POINT('Origin',(1.6,-4.5,6.15));
#20763=CARTESIAN_POINT('',(1.2,-4.5,6.5));
#20764=CARTESIAN_POINT('Origin',(1.6,-4.5,6.15));
#20765=CARTESIAN_POINT('Origin',(0.5,-4.5,6.15));
#20766=CARTESIAN_POINT('',(0.5,-4.5,6.35));
#20767=CARTESIAN_POINT('',(0.5,-4.5,6.35));
#20768=CARTESIAN_POINT('Origin',(0.5,-4.5,6.15));
#20769=CARTESIAN_POINT('Origin',(0.5,-4.5,6.15));
#20770=CARTESIAN_POINT('',(0.,0.,0.));
#20771=CARTESIAN_POINT('Origin',(-10.,-7.,8.));
#20772=CARTESIAN_POINT('',(1.,-7.,8.6));
#20773=CARTESIAN_POINT('Origin',(1.,-7.,8.));
#20774=CARTESIAN_POINT('',(-10.,-7.,8.6));
#20775=CARTESIAN_POINT('',(-10.,-7.,8.6));
#20776=CARTESIAN_POINT('Origin',(-10.,-7.,8.));
#20777=CARTESIAN_POINT('Origin',(1.,-7.,8.));
#20778=CARTESIAN_POINT('Origin',(-10.,-7.,8.));
#20779=CARTESIAN_POINT('',(0.,0.,0.));
#20780=CARTESIAN_POINT('Origin',(-10.,-2.,8.));
#20781=CARTESIAN_POINT('',(1.,-2.,8.6));
#20782=CARTESIAN_POINT('Origin',(1.,-2.,8.));
#20783=CARTESIAN_POINT('',(-10.,-2.,8.6));
#20784=CARTESIAN_POINT('',(-10.,-2.,8.6));
#20785=CARTESIAN_POINT('Origin',(-10.,-2.,8.));
#20786=CARTESIAN_POINT('Origin',(1.,-2.,8.));
#20787=CARTESIAN_POINT('Origin',(-10.,-2.,8.));
#20788=CARTESIAN_POINT('',(0.,0.,0.));
#20789=CARTESIAN_POINT('Origin',(0.375,0.5,0.));
#20790=CARTESIAN_POINT('',(-0.375,0.5,-4.59242549680257E-17));
#20791=CARTESIAN_POINT('Origin',(0.,0.5,0.));
#20792=CARTESIAN_POINT('Origin',(0.,0.475,0.));
#20793=CARTESIAN_POINT('',(-0.425,0.45,-5.20474889637625E-17));
#20794=CARTESIAN_POINT('Origin',(0.,0.45,0.));
#20795=CARTESIAN_POINT('',(-0.4,0.475,-4.89858719658941E-17));
#20796=CARTESIAN_POINT('Origin',(0.,0.24,0.));
#20797=CARTESIAN_POINT('',(-0.425,0.0299999999999998,-5.20474889637625E-17));
#20798=CARTESIAN_POINT('Origin',(0.,0.0299999999999998,0.));
#20799=CARTESIAN_POINT('',(-0.425,0.24,-5.20474889637625E-17));
#20800=CARTESIAN_POINT('Origin',(0.,0.0150000000000001,0.));
#20801=CARTESIAN_POINT('',(-0.395,4.85722573273506E-17,-4.83735485663204E-17));
#20802=CARTESIAN_POINT('Origin',(0.,0.,0.));
#20803=CARTESIAN_POINT('',(-0.41,0.0150000000000001,-5.02105187650415E-17));
#20804=CARTESIAN_POINT('Origin',(0.27,0.,0.));
#20805=CARTESIAN_POINT('',(-0.27,0.,-3.30654635769785E-17));
#20806=CARTESIAN_POINT('Origin',(0.,0.,0.));
#20807=CARTESIAN_POINT('Origin',(0.,-0.02,0.));
#20808=CARTESIAN_POINT('',(-0.24505,-0.0498999999999999,3.00099698131059E-17));
#20809=CARTESIAN_POINT('Origin',(0.,-0.0498999999999999,0.));
#20810=CARTESIAN_POINT('',(-0.26,-0.02,-3.18408167778312E-17));
#20811=CARTESIAN_POINT('Origin',(0.,-0.995,0.));
#20812=CARTESIAN_POINT('',(-0.24505,-1.95495,3.00099698131059E-17));
#20813=CARTESIAN_POINT('Origin',(0.,-1.95495,0.));
#20814=CARTESIAN_POINT('',(-0.24505,-0.995,-3.00099698131059E-17));
#20815=CARTESIAN_POINT('Origin',(0.,-1.975,0.));
#20816=CARTESIAN_POINT('',(-0.2,-2.,-2.44929359829471E-17));
#20817=CARTESIAN_POINT('Origin',(0.,-2.,0.));
#20818=CARTESIAN_POINT('',(-0.225,-1.975,-2.75545529808154E-17));
#20819=CARTESIAN_POINT('Origin',(0.,-2.,0.));
#20820=CARTESIAN_POINT('Origin',(0.115470053837925,-0.5,-0.2));
#20821=CARTESIAN_POINT('',(0.23094010767585,-0.5,0.));
#20822=CARTESIAN_POINT('',(0.115470053837925,-0.5,-0.2));
#20823=CARTESIAN_POINT('',(0.23094010767585,-0.5,0.));
#20824=CARTESIAN_POINT('',(0.115470053837925,-0.8,-0.2));
#20825=CARTESIAN_POINT('',(0.115470053837925,-0.5,-0.2));
#20826=CARTESIAN_POINT('',(0.23094010767585,-0.8,0.));
#20827=CARTESIAN_POINT('',(0.23094010767585,-0.8,0.));
#20828=CARTESIAN_POINT('',(0.23094010767585,-0.5,0.));
#20829=CARTESIAN_POINT('Origin',(-0.115470053837925,-0.5,-0.2));
#20830=CARTESIAN_POINT('',(-0.115470053837925,-0.5,-0.2));
#20831=CARTESIAN_POINT('',(0.115470053837925,-0.5,-0.2));
#20832=CARTESIAN_POINT('',(-0.115470053837925,-0.8,-0.2));
#20833=CARTESIAN_POINT('',(-0.115470053837925,-0.5,-0.2));
#20834=CARTESIAN_POINT('',(0.115470053837925,-0.8,-0.2));
#20835=CARTESIAN_POINT('Origin',(-0.23094010767585,-0.5,-2.77555756156289E-17));
#20836=CARTESIAN_POINT('',(-0.23094010767585,-0.5,-2.82820063659975E-17));
#20837=CARTESIAN_POINT('',(-0.115470053837925,-0.5,-0.2));
#20838=CARTESIAN_POINT('',(-0.23094010767585,-0.8,-2.77555756156289E-17));
#20839=CARTESIAN_POINT('',(-0.23094010767585,-0.5,-2.82820063659975E-17));
#20840=CARTESIAN_POINT('',(-0.115470053837925,-0.8,-0.2));
#20841=CARTESIAN_POINT('Origin',(-0.115470053837925,-0.5,0.2));
#20842=CARTESIAN_POINT('',(-0.115470053837925,-0.5,0.2));
#20843=CARTESIAN_POINT('',(-0.23094010767585,-0.5,-2.82820063659975E-17));
#20844=CARTESIAN_POINT('',(-0.115470053837925,-0.8,0.2));
#20845=CARTESIAN_POINT('',(-0.115470053837925,-0.5,0.2));
#20846=CARTESIAN_POINT('',(-0.23094010767585,-0.8,-2.82820063659975E-17));
#20847=CARTESIAN_POINT('Origin',(0.115470053837925,-0.5,0.2));
#20848=CARTESIAN_POINT('',(0.115470053837925,-0.5,0.2));
#20849=CARTESIAN_POINT('',(-0.115470053837925,-0.5,0.2));
#20850=CARTESIAN_POINT('',(0.115470053837925,-0.8,0.2));
#20851=CARTESIAN_POINT('',(0.115470053837925,-0.5,0.2));
#20852=CARTESIAN_POINT('',(-0.115470053837925,-0.8,0.2));
#20853=CARTESIAN_POINT('Origin',(0.23094010767585,-0.5,0.));
#20854=CARTESIAN_POINT('',(0.115470053837925,-0.5,0.2));
#20855=CARTESIAN_POINT('',(0.115470053837925,-0.8,0.2));
#20856=CARTESIAN_POINT('Origin',(0.,-0.5,0.));
#20857=CARTESIAN_POINT('Origin',(0.,-0.8,0.));
#20858=CARTESIAN_POINT('',(0.,0.,0.));
#20859=CARTESIAN_POINT('',(0.,0.,0.));
#20860=CARTESIAN_POINT('Origin',(8.08877866266397,-0.6,17.1120538880616));
#20861=CARTESIAN_POINT('',(7.92377866266397,-0.5,17.1120538880616));
#20862=CARTESIAN_POINT('Origin',(8.08877866266397,-0.5,17.1120538880616));
#20863=CARTESIAN_POINT('',(7.92377866266397,0.5,17.1120538880616));
#20864=CARTESIAN_POINT('',(7.92377866266397,-0.6,17.1120538880616));
#20865=CARTESIAN_POINT('Origin',(8.08877866266397,0.5,17.1120538880616));
#20866=CARTESIAN_POINT('Origin',(8.08877866266397,-0.6,19.7283489784518));
#20867=CARTESIAN_POINT('',(7.92377866266397,-0.5,19.7283489784518));
#20868=CARTESIAN_POINT('Origin',(8.08877866266397,-0.5,19.7283489784518));
#20869=CARTESIAN_POINT('',(7.92377866266397,0.5,19.7283489784518));
#20870=CARTESIAN_POINT('',(7.92377866266397,-0.6,19.7283489784518));
#20871=CARTESIAN_POINT('Origin',(8.08877866266397,0.5,19.7283489784518));
#20872=CARTESIAN_POINT('Origin',(10.7050737530542,-0.6,19.7283489784518));
#20873=CARTESIAN_POINT('',(10.5400737530542,-0.5,19.7283489784518));
#20874=CARTESIAN_POINT('Origin',(10.7050737530542,-0.5,19.7283489784518));
#20875=CARTESIAN_POINT('',(10.5400737530542,0.5,19.7283489784518));
#20876=CARTESIAN_POINT('',(10.5400737530542,-0.6,19.7283489784518));
#20877=CARTESIAN_POINT('Origin',(10.7050737530542,0.5,19.7283489784518));
#20878=CARTESIAN_POINT('Origin',(10.7050737530542,-0.6,17.1120538880616));
#20879=CARTESIAN_POINT('',(10.5400737530542,-0.5,17.1120538880616));
#20880=CARTESIAN_POINT('Origin',(10.7050737530542,-0.5,17.1120538880616));
#20881=CARTESIAN_POINT('',(10.5400737530542,0.5,17.1120538880616));
#20882=CARTESIAN_POINT('',(10.5400737530542,-0.6,17.1120538880616));
#20883=CARTESIAN_POINT('Origin',(10.7050737530542,0.5,17.1120538880616));
#20884=CARTESIAN_POINT('Origin',(9.39692620785909,-0.6,18.4202014332567));
#20885=CARTESIAN_POINT('',(7.79692620785909,-0.5,18.4202014332567));
#20886=CARTESIAN_POINT('Origin',(9.39692620785909,-0.5,18.4202014332567));
#20887=CARTESIAN_POINT('',(7.79692620785909,0.5,18.4202014332567));
#20888=CARTESIAN_POINT('',(7.79692620785909,-0.6,18.4202014332567));
#20889=CARTESIAN_POINT('Origin',(9.39692620785909,0.5,18.4202014332567));
#20890=CARTESIAN_POINT('Origin',(9.39692620785909,-0.5,18.4202014332567));
#20891=CARTESIAN_POINT('',(7.81832456572892,0.5,16.8878774285292));
#20892=CARTESIAN_POINT('',(7.81832456572892,-0.5,16.8878774285292));
#20893=CARTESIAN_POINT('',(7.81832456572892,-0.5,16.8878774285292));
#20894=CARTESIAN_POINT('',(7.20268830774272,0.5,18.5793241459439));
#20895=CARTESIAN_POINT('Origin',(9.39692620785909,0.5,18.4202014332567));
#20896=CARTESIAN_POINT('',(7.20268830774272,-0.5,18.5793241459439));
#20897=CARTESIAN_POINT('',(7.20268830774272,-0.5,18.5793241459439));
#20898=CARTESIAN_POINT('Origin',(9.39692620785909,-0.5,18.4202014332567));
#20899=CARTESIAN_POINT('Origin',(4.69846310392954,-0.5,16.7101007166283));
#20900=CARTESIAN_POINT('',(1.57860164213016,-0.5,16.5323240047274));
#20901=CARTESIAN_POINT('',(-0.307818128993102,-0.5,15.8457233587073));
#20902=CARTESIAN_POINT('',(2.19423790011636,-0.5,14.8408772873128));
#20903=CARTESIAN_POINT('Origin',(0.,-0.5,15.));
#20904=CARTESIAN_POINT('',(9.70474433685219,-0.5,17.5744780745494));
#20905=CARTESIAN_POINT('',(-1.6,-0.5,15.));
#20906=CARTESIAN_POINT('Origin',(0.,-0.5,15.));
#20907=CARTESIAN_POINT('',(1.14314754519511,-0.5,13.6918524548049));
#20908=CARTESIAN_POINT('Origin',(1.30814754519511,-0.5,13.6918524548049));
#20909=CARTESIAN_POINT('',(1.14314754519511,-0.5,16.3081475451951));
#20910=CARTESIAN_POINT('Origin',(1.30814754519511,-0.5,16.3081475451951));
#20911=CARTESIAN_POINT('',(-1.47314754519511,-0.5,16.3081475451951));
#20912=CARTESIAN_POINT('Origin',(-1.30814754519511,-0.5,16.3081475451951));
#20913=CARTESIAN_POINT('',(-1.47314754519511,-0.5,13.6918524548049));
#20914=CARTESIAN_POINT('Origin',(-1.30814754519511,-0.5,13.6918524548049));
#20915=CARTESIAN_POINT('Origin',(-0.307818128993102,-0.5,15.8457233587073));
#20916=CARTESIAN_POINT('',(1.57860164213016,0.5,16.5323240047274));
#20917=CARTESIAN_POINT('',(-0.307818128993102,0.5,15.8457233587073));
#20918=CARTESIAN_POINT('',(1.57860164213016,-0.5,16.5323240047274));
#20919=CARTESIAN_POINT('Origin',(-1.30814754519511,-0.6,13.6918524548049));
#20920=CARTESIAN_POINT('',(-1.47314754519511,0.5,13.6918524548049));
#20921=CARTESIAN_POINT('',(-1.47314754519511,-0.6,13.6918524548049));
#20922=CARTESIAN_POINT('Origin',(-1.30814754519511,0.5,13.6918524548049));
#20923=CARTESIAN_POINT('Origin',(-1.30814754519511,-0.6,16.3081475451951));
#20924=CARTESIAN_POINT('',(-1.47314754519511,0.5,16.3081475451951));
#20925=CARTESIAN_POINT('',(-1.47314754519511,-0.6,16.3081475451951));
#20926=CARTESIAN_POINT('Origin',(-1.30814754519511,0.5,16.3081475451951));
#20927=CARTESIAN_POINT('Origin',(1.30814754519511,-0.6,16.3081475451951));
#20928=CARTESIAN_POINT('',(1.14314754519511,0.5,16.3081475451951));
#20929=CARTESIAN_POINT('',(1.14314754519511,-0.6,16.3081475451951));
#20930=CARTESIAN_POINT('Origin',(1.30814754519511,0.5,16.3081475451951));
#20931=CARTESIAN_POINT('Origin',(1.30814754519511,-0.6,13.6918524548049));
#20932=CARTESIAN_POINT('',(1.14314754519511,0.5,13.6918524548049));
#20933=CARTESIAN_POINT('',(1.14314754519511,-0.6,13.6918524548049));
#20934=CARTESIAN_POINT('Origin',(1.30814754519511,0.5,13.6918524548049));
#20935=CARTESIAN_POINT('Origin',(0.,-0.6,15.));
#20936=CARTESIAN_POINT('',(-1.6,0.5,15.));
#20937=CARTESIAN_POINT('',(-1.6,-0.6,15.));
#20938=CARTESIAN_POINT('Origin',(0.,0.5,15.));
#20939=CARTESIAN_POINT('Origin',(0.,-0.5,15.));
#20940=CARTESIAN_POINT('',(2.19423790011636,0.5,14.8408772873128));
#20941=CARTESIAN_POINT('',(2.19423790011636,-0.5,14.8408772873128));
#20942=CARTESIAN_POINT('Origin',(0.,0.5,15.));
#20943=CARTESIAN_POINT('Origin',(9.70474433685219,-0.5,17.5744780745494));
#20944=CARTESIAN_POINT('',(9.70474433685219,0.5,17.5744780745494));
#20945=CARTESIAN_POINT('Origin',(4.69846310392954,0.5,16.7101007166283));
#20946=CARTESIAN_POINT('',(0.,0.,0.));
#20947=CARTESIAN_POINT('Origin',(-1.30814754519511,-0.9,13.6918524548049));
#20948=CARTESIAN_POINT('',(-1.53314754519511,-0.8,13.6918524548049));
#20949=CARTESIAN_POINT('Origin',(-1.30814754519511,-0.8,13.6918524548049));
#20950=CARTESIAN_POINT('',(-1.53314754519511,-0.5,13.6918524548049));
#20951=CARTESIAN_POINT('',(-1.53314754519511,-0.9,13.6918524548049));
#20952=CARTESIAN_POINT('Origin',(-1.30814754519511,-0.5,13.6918524548049));
#20953=CARTESIAN_POINT('Origin',(-1.30814754519511,-0.9,16.3081475451951));
#20954=CARTESIAN_POINT('',(-1.53314754519511,-0.8,16.3081475451951));
#20955=CARTESIAN_POINT('Origin',(-1.30814754519511,-0.8,16.3081475451951));
#20956=CARTESIAN_POINT('',(-1.53314754519511,-0.5,16.3081475451951));
#20957=CARTESIAN_POINT('',(-1.53314754519511,-0.9,16.3081475451951));
#20958=CARTESIAN_POINT('Origin',(-1.30814754519511,-0.5,16.3081475451951));
#20959=CARTESIAN_POINT('Origin',(1.30814754519511,-0.9,16.3081475451951));
#20960=CARTESIAN_POINT('',(1.08314754519511,-0.8,16.3081475451951));
#20961=CARTESIAN_POINT('Origin',(1.30814754519511,-0.8,16.3081475451951));
#20962=CARTESIAN_POINT('',(1.08314754519511,-0.5,16.3081475451951));
#20963=CARTESIAN_POINT('',(1.08314754519511,-0.9,16.3081475451951));
#20964=CARTESIAN_POINT('Origin',(1.30814754519511,-0.5,16.3081475451951));
#20965=CARTESIAN_POINT('Origin',(1.30814754519511,-0.9,13.6918524548049));
#20966=CARTESIAN_POINT('',(1.08314754519511,-0.8,13.6918524548049));
#20967=CARTESIAN_POINT('Origin',(1.30814754519511,-0.8,13.6918524548049));
#20968=CARTESIAN_POINT('',(1.08314754519511,-0.5,13.6918524548049));
#20969=CARTESIAN_POINT('',(1.08314754519511,-0.9,13.6918524548049));
#20970=CARTESIAN_POINT('Origin',(1.30814754519511,-0.5,13.6918524548049));
#20971=CARTESIAN_POINT('Origin',(0.,-0.8,15.));
#20972=CARTESIAN_POINT('',(-1.02,-0.5,15.));
#20973=CARTESIAN_POINT('Origin',(0.,-0.5,15.));
#20974=CARTESIAN_POINT('',(-1.02,-0.8,15.));
#20975=CARTESIAN_POINT('',(-1.02,-0.8,15.));
#20976=CARTESIAN_POINT('Origin',(0.,-0.8,15.));
#20977=CARTESIAN_POINT('Origin',(0.,-0.8,15.));
#20978=CARTESIAN_POINT('',(-2.2,-0.5,15.));
#20979=CARTESIAN_POINT('Origin',(0.,-0.5,15.));
#20980=CARTESIAN_POINT('',(-2.2,-0.8,15.));
#20981=CARTESIAN_POINT('',(-2.2,-0.8,15.));
#20982=CARTESIAN_POINT('Origin',(0.,-0.8,15.));
#20983=CARTESIAN_POINT('Origin',(0.,-0.5,15.));
#20984=CARTESIAN_POINT('Origin',(0.,-0.8,15.));
#20985=CARTESIAN_POINT('',(0.,0.,0.));
#20986=CARTESIAN_POINT('Origin',(1.30814754519511,-0.8,16.3081475451951));
#20987=CARTESIAN_POINT('',(0.958147545195113,-0.8,16.3081475451951));
#20988=CARTESIAN_POINT('Origin',(1.30814754519511,-0.8,16.3081475451951));
#20989=CARTESIAN_POINT('',(1.10814754519511,-0.8,16.3081475451951));
#20990=CARTESIAN_POINT('Origin',(1.30814754519511,-0.8,16.3081475451951));
#20991=CARTESIAN_POINT('Origin',(1.30814754519511,-1.2,16.3081475451951));
#20992=CARTESIAN_POINT('',(0.958147545195113,-1.2,16.3081475451951));
#20993=CARTESIAN_POINT('',(0.958147545195113,-1.2,16.3081475451951));
#20994=CARTESIAN_POINT('Origin',(1.30814754519511,-1.2,16.3081475451951));
#20995=CARTESIAN_POINT('Origin',(1.30814754519511,-1.2,16.3081475451951));
#20996=CARTESIAN_POINT('Origin',(1.30814754519511,-0.8,16.3081475451951));
#20997=CARTESIAN_POINT('',(1.10814754519511,-0.1,16.3081475451951));
#20998=CARTESIAN_POINT('Origin',(1.30814754519511,-0.1,16.3081475451951));
#20999=CARTESIAN_POINT('',(1.10814754519511,-0.8,16.3081475451951));
#21000=CARTESIAN_POINT('Origin',(1.30814754519511,-0.1,16.3081475451951));
#21001=CARTESIAN_POINT('',(0.,0.,0.));
#21002=CARTESIAN_POINT('Origin',(-1.30814754519511,-0.8,16.3081475451951));
#21003=CARTESIAN_POINT('',(-1.65814754519511,-0.8,16.3081475451951));
#21004=CARTESIAN_POINT('Origin',(-1.30814754519511,-0.8,16.3081475451951));
#21005=CARTESIAN_POINT('',(-1.50814754519511,-0.8,16.3081475451951));
#21006=CARTESIAN_POINT('Origin',(-1.30814754519511,-0.8,16.3081475451951));
#21007=CARTESIAN_POINT('Origin',(-1.30814754519511,-1.2,16.3081475451951));
#21008=CARTESIAN_POINT('',(-1.65814754519511,-1.2,16.3081475451951));
#21009=CARTESIAN_POINT('',(-1.65814754519511,-1.2,16.3081475451951));
#21010=CARTESIAN_POINT('Origin',(-1.30814754519511,-1.2,16.3081475451951));
#21011=CARTESIAN_POINT('Origin',(-1.30814754519511,-1.2,16.3081475451951));
#21012=CARTESIAN_POINT('Origin',(-1.30814754519511,-0.8,16.3081475451951));
#21013=CARTESIAN_POINT('',(-1.50814754519511,-0.1,16.3081475451951));
#21014=CARTESIAN_POINT('Origin',(-1.30814754519511,-0.1,16.3081475451951));
#21015=CARTESIAN_POINT('',(-1.50814754519511,-0.8,16.3081475451951));
#21016=CARTESIAN_POINT('Origin',(-1.30814754519511,-0.1,16.3081475451951));
#21017=CARTESIAN_POINT('',(0.,0.,0.));
#21018=CARTESIAN_POINT('Origin',(-1.30814754519511,-0.8,13.6918524548049));
#21019=CARTESIAN_POINT('',(-1.65814754519511,-0.8,13.6918524548049));
#21020=CARTESIAN_POINT('Origin',(-1.30814754519511,-0.8,13.6918524548049));
#21021=CARTESIAN_POINT('',(-1.50814754519511,-0.8,13.6918524548049));
#21022=CARTESIAN_POINT('Origin',(-1.30814754519511,-0.8,13.6918524548049));
#21023=CARTESIAN_POINT('Origin',(-1.30814754519511,-1.2,13.6918524548049));
#21024=CARTESIAN_POINT('',(-1.65814754519511,-1.2,13.6918524548049));
#21025=CARTESIAN_POINT('',(-1.65814754519511,-1.2,13.6918524548049));
#21026=CARTESIAN_POINT('Origin',(-1.30814754519511,-1.2,13.6918524548049));
#21027=CARTESIAN_POINT('Origin',(-1.30814754519511,-1.2,13.6918524548049));
#21028=CARTESIAN_POINT('Origin',(-1.30814754519511,-0.8,13.6918524548049));
#21029=CARTESIAN_POINT('',(-1.50814754519511,-0.1,13.6918524548049));
#21030=CARTESIAN_POINT('Origin',(-1.30814754519511,-0.1,13.6918524548049));
#21031=CARTESIAN_POINT('',(-1.50814754519511,-0.8,13.6918524548049));
#21032=CARTESIAN_POINT('Origin',(-1.30814754519511,-0.1,13.6918524548049));
#21033=CARTESIAN_POINT('',(0.,0.,0.));
#21034=CARTESIAN_POINT('Origin',(1.30814754519511,-0.8,13.6918524548049));
#21035=CARTESIAN_POINT('',(0.958147545195112,-0.8,13.6918524548049));
#21036=CARTESIAN_POINT('Origin',(1.30814754519511,-0.8,13.6918524548049));
#21037=CARTESIAN_POINT('',(1.10814754519511,-0.8,13.6918524548049));
#21038=CARTESIAN_POINT('Origin',(1.30814754519511,-0.8,13.6918524548049));
#21039=CARTESIAN_POINT('Origin',(1.30814754519511,-1.2,13.6918524548049));
#21040=CARTESIAN_POINT('',(0.958147545195112,-1.2,13.6918524548049));
#21041=CARTESIAN_POINT('',(0.958147545195112,-1.2,13.6918524548049));
#21042=CARTESIAN_POINT('Origin',(1.30814754519511,-1.2,13.6918524548049));
#21043=CARTESIAN_POINT('Origin',(1.30814754519511,-1.2,13.6918524548049));
#21044=CARTESIAN_POINT('Origin',(1.30814754519511,-0.8,13.6918524548049));
#21045=CARTESIAN_POINT('',(1.10814754519511,-0.1,13.6918524548049));
#21046=CARTESIAN_POINT('Origin',(1.30814754519511,-0.1,13.6918524548049));
#21047=CARTESIAN_POINT('',(1.10814754519511,-0.8,13.6918524548049));
#21048=CARTESIAN_POINT('Origin',(1.30814754519511,-0.1,13.6918524548049));
#21049=CARTESIAN_POINT('',(0.,0.,0.));
#21050=CARTESIAN_POINT('Origin',(-1.30814754519511,0.4,13.6918524548049));
#21051=CARTESIAN_POINT('',(-1.53314754519511,0.5,13.6918524548049));
#21052=CARTESIAN_POINT('Origin',(-1.30814754519511,0.5,13.6918524548049));
#21053=CARTESIAN_POINT('',(-1.53314754519511,0.8,13.6918524548049));
#21054=CARTESIAN_POINT('',(-1.53314754519511,0.4,13.6918524548049));
#21055=CARTESIAN_POINT('Origin',(-1.30814754519511,0.8,13.6918524548049));
#21056=CARTESIAN_POINT('Origin',(-1.30814754519511,0.4,16.3081475451951));
#21057=CARTESIAN_POINT('',(-1.53314754519511,0.5,16.3081475451951));
#21058=CARTESIAN_POINT('Origin',(-1.30814754519511,0.5,16.3081475451951));
#21059=CARTESIAN_POINT('',(-1.53314754519511,0.8,16.3081475451951));
#21060=CARTESIAN_POINT('',(-1.53314754519511,0.4,16.3081475451951));
#21061=CARTESIAN_POINT('Origin',(-1.30814754519511,0.8,16.3081475451951));
#21062=CARTESIAN_POINT('Origin',(1.30814754519511,0.4,16.3081475451951));
#21063=CARTESIAN_POINT('',(1.08314754519511,0.5,16.3081475451951));
#21064=CARTESIAN_POINT('Origin',(1.30814754519511,0.5,16.3081475451951));
#21065=CARTESIAN_POINT('',(1.08314754519511,0.8,16.3081475451951));
#21066=CARTESIAN_POINT('',(1.08314754519511,0.4,16.3081475451951));
#21067=CARTESIAN_POINT('Origin',(1.30814754519511,0.8,16.3081475451951));
#21068=CARTESIAN_POINT('Origin',(1.30814754519511,0.4,13.6918524548049));
#21069=CARTESIAN_POINT('',(1.08314754519511,0.5,13.6918524548049));
#21070=CARTESIAN_POINT('Origin',(1.30814754519511,0.5,13.6918524548049));
#21071=CARTESIAN_POINT('',(1.08314754519511,0.8,13.6918524548049));
#21072=CARTESIAN_POINT('',(1.08314754519511,0.4,13.6918524548049));
#21073=CARTESIAN_POINT('Origin',(1.30814754519511,0.8,13.6918524548049));
#21074=CARTESIAN_POINT('Origin',(0.,0.5,15.));
#21075=CARTESIAN_POINT('',(-1.02,0.8,15.));
#21076=CARTESIAN_POINT('Origin',(0.,0.8,15.));
#21077=CARTESIAN_POINT('',(-1.02,0.5,15.));
#21078=CARTESIAN_POINT('',(-1.02,0.5,15.));
#21079=CARTESIAN_POINT('Origin',(0.,0.5,15.));
#21080=CARTESIAN_POINT('Origin',(0.,0.5,15.));
#21081=CARTESIAN_POINT('',(-2.2,0.8,15.));
#21082=CARTESIAN_POINT('Origin',(0.,0.8,15.));
#21083=CARTESIAN_POINT('',(-2.2,0.5,15.));
#21084=CARTESIAN_POINT('',(-2.2,0.5,15.));
#21085=CARTESIAN_POINT('Origin',(0.,0.5,15.));
#21086=CARTESIAN_POINT('Origin',(0.,0.8,15.));
#21087=CARTESIAN_POINT('Origin',(0.,0.5,15.));
#21088=CARTESIAN_POINT('',(0.,0.,0.));
#21089=CARTESIAN_POINT('Origin',(1.30814754519511,0.8,16.3081475451951));
#21090=CARTESIAN_POINT('',(0.958147545195113,0.8,16.3081475451951));
#21091=CARTESIAN_POINT('Origin',(1.30814754519511,0.8,16.3081475451951));
#21092=CARTESIAN_POINT('',(1.10814754519511,0.8,16.3081475451951));
#21093=CARTESIAN_POINT('Origin',(1.30814754519511,0.8,16.3081475451951));
#21094=CARTESIAN_POINT('Origin',(1.30814754519511,0.8,16.3081475451951));
#21095=CARTESIAN_POINT('',(0.958147545195113,1.2,16.3081475451951));
#21096=CARTESIAN_POINT('Origin',(1.30814754519511,1.2,16.3081475451951));
#21097=CARTESIAN_POINT('',(0.958147545195113,0.8,16.3081475451951));
#21098=CARTESIAN_POINT('Origin',(1.30814754519511,1.2,16.3081475451951));
#21099=CARTESIAN_POINT('Origin',(1.30814754519511,0.1,16.3081475451951));
#21100=CARTESIAN_POINT('',(1.10814754519511,0.1,16.3081475451951));
#21101=CARTESIAN_POINT('',(1.10814754519511,0.1,16.3081475451951));
#21102=CARTESIAN_POINT('Origin',(1.30814754519511,0.1,16.3081475451951));
#21103=CARTESIAN_POINT('Origin',(1.30814754519511,0.1,16.3081475451951));
#21104=CARTESIAN_POINT('',(0.,0.,0.));
#21105=CARTESIAN_POINT('Origin',(-1.30814754519511,0.8,16.3081475451951));
#21106=CARTESIAN_POINT('',(-1.65814754519511,0.8,16.3081475451951));
#21107=CARTESIAN_POINT('Origin',(-1.30814754519511,0.8,16.3081475451951));
#21108=CARTESIAN_POINT('',(-1.50814754519511,0.8,16.3081475451951));
#21109=CARTESIAN_POINT('Origin',(-1.30814754519511,0.8,16.3081475451951));
#21110=CARTESIAN_POINT('Origin',(-1.30814754519511,0.8,16.3081475451951));
#21111=CARTESIAN_POINT('',(-1.65814754519511,1.2,16.3081475451951));
#21112=CARTESIAN_POINT('Origin',(-1.30814754519511,1.2,16.3081475451951));
#21113=CARTESIAN_POINT('',(-1.65814754519511,0.8,16.3081475451951));
#21114=CARTESIAN_POINT('Origin',(-1.30814754519511,1.2,16.3081475451951));
#21115=CARTESIAN_POINT('Origin',(-1.30814754519511,0.1,16.3081475451951));
#21116=CARTESIAN_POINT('',(-1.50814754519511,0.1,16.3081475451951));
#21117=CARTESIAN_POINT('',(-1.50814754519511,0.1,16.3081475451951));
#21118=CARTESIAN_POINT('Origin',(-1.30814754519511,0.1,16.3081475451951));
#21119=CARTESIAN_POINT('Origin',(-1.30814754519511,0.1,16.3081475451951));
#21120=CARTESIAN_POINT('',(0.,0.,0.));
#21121=CARTESIAN_POINT('Origin',(-1.30814754519511,0.8,13.6918524548049));
#21122=CARTESIAN_POINT('',(-1.65814754519511,0.8,13.6918524548049));
#21123=CARTESIAN_POINT('Origin',(-1.30814754519511,0.8,13.6918524548049));
#21124=CARTESIAN_POINT('',(-1.50814754519511,0.8,13.6918524548049));
#21125=CARTESIAN_POINT('Origin',(-1.30814754519511,0.8,13.6918524548049));
#21126=CARTESIAN_POINT('Origin',(-1.30814754519511,0.8,13.6918524548049));
#21127=CARTESIAN_POINT('',(-1.65814754519511,1.2,13.6918524548049));
#21128=CARTESIAN_POINT('Origin',(-1.30814754519511,1.2,13.6918524548049));
#21129=CARTESIAN_POINT('',(-1.65814754519511,0.8,13.6918524548049));
#21130=CARTESIAN_POINT('Origin',(-1.30814754519511,1.2,13.6918524548049));
#21131=CARTESIAN_POINT('Origin',(-1.30814754519511,0.1,13.6918524548049));
#21132=CARTESIAN_POINT('',(-1.50814754519511,0.1,13.6918524548049));
#21133=CARTESIAN_POINT('',(-1.50814754519511,0.1,13.6918524548049));
#21134=CARTESIAN_POINT('Origin',(-1.30814754519511,0.1,13.6918524548049));
#21135=CARTESIAN_POINT('Origin',(-1.30814754519511,0.1,13.6918524548049));
#21136=CARTESIAN_POINT('',(0.,0.,0.));
#21137=CARTESIAN_POINT('Origin',(1.30814754519511,0.8,13.6918524548049));
#21138=CARTESIAN_POINT('',(0.958147545195112,0.8,13.6918524548049));
#21139=CARTESIAN_POINT('Origin',(1.30814754519511,0.8,13.6918524548049));
#21140=CARTESIAN_POINT('',(1.10814754519511,0.8,13.6918524548049));
#21141=CARTESIAN_POINT('Origin',(1.30814754519511,0.8,13.6918524548049));
#21142=CARTESIAN_POINT('Origin',(1.30814754519511,0.8,13.6918524548049));
#21143=CARTESIAN_POINT('',(0.958147545195112,1.2,13.6918524548049));
#21144=CARTESIAN_POINT('Origin',(1.30814754519511,1.2,13.6918524548049));
#21145=CARTESIAN_POINT('',(0.958147545195112,0.8,13.6918524548049));
#21146=CARTESIAN_POINT('Origin',(1.30814754519511,1.2,13.6918524548049));
#21147=CARTESIAN_POINT('Origin',(1.30814754519511,0.1,13.6918524548049));
#21148=CARTESIAN_POINT('',(1.10814754519511,0.1,13.6918524548049));
#21149=CARTESIAN_POINT('',(1.10814754519511,0.1,13.6918524548049));
#21150=CARTESIAN_POINT('Origin',(1.30814754519511,0.1,13.6918524548049));
#21151=CARTESIAN_POINT('Origin',(1.30814754519511,0.1,13.6918524548049));
#21152=CARTESIAN_POINT('',(0.,0.,0.));
#21153=CARTESIAN_POINT('Origin',(8.08877866266397,-0.9,17.1120538880616));
#21154=CARTESIAN_POINT('',(7.86377866266397,-0.8,17.1120538880616));
#21155=CARTESIAN_POINT('Origin',(8.08877866266397,-0.8,17.1120538880616));
#21156=CARTESIAN_POINT('',(7.86377866266397,-0.5,17.1120538880616));
#21157=CARTESIAN_POINT('',(7.86377866266397,-0.9,17.1120538880616));
#21158=CARTESIAN_POINT('Origin',(8.08877866266397,-0.5,17.1120538880616));
#21159=CARTESIAN_POINT('Origin',(8.08877866266397,-0.9,19.7283489784518));
#21160=CARTESIAN_POINT('',(7.86377866266397,-0.8,19.7283489784518));
#21161=CARTESIAN_POINT('Origin',(8.08877866266397,-0.8,19.7283489784518));
#21162=CARTESIAN_POINT('',(7.86377866266397,-0.5,19.7283489784518));
#21163=CARTESIAN_POINT('',(7.86377866266397,-0.9,19.7283489784518));
#21164=CARTESIAN_POINT('Origin',(8.08877866266397,-0.5,19.7283489784518));
#21165=CARTESIAN_POINT('Origin',(10.7050737530542,-0.9,19.7283489784518));
#21166=CARTESIAN_POINT('',(10.4800737530542,-0.8,19.7283489784518));
#21167=CARTESIAN_POINT('Origin',(10.7050737530542,-0.8,19.7283489784518));
#21168=CARTESIAN_POINT('',(10.4800737530542,-0.5,19.7283489784518));
#21169=CARTESIAN_POINT('',(10.4800737530542,-0.9,19.7283489784518));
#21170=CARTESIAN_POINT('Origin',(10.7050737530542,-0.5,19.7283489784518));
#21171=CARTESIAN_POINT('Origin',(10.7050737530542,-0.9,17.1120538880616));
#21172=CARTESIAN_POINT('',(10.4800737530542,-0.8,17.1120538880616));
#21173=CARTESIAN_POINT('Origin',(10.7050737530542,-0.8,17.1120538880616));
#21174=CARTESIAN_POINT('',(10.4800737530542,-0.5,17.1120538880616));
#21175=CARTESIAN_POINT('',(10.4800737530542,-0.9,17.1120538880616));
#21176=CARTESIAN_POINT('Origin',(10.7050737530542,-0.5,17.1120538880616));
#21177=CARTESIAN_POINT('Origin',(9.39692620785909,-0.8,18.4202014332567));
#21178=CARTESIAN_POINT('',(8.37692620785909,-0.5,18.4202014332567));
#21179=CARTESIAN_POINT('Origin',(9.39692620785909,-0.5,18.4202014332567));
#21180=CARTESIAN_POINT('',(8.37692620785909,-0.8,18.4202014332567));
#21181=CARTESIAN_POINT('',(8.37692620785909,-0.8,18.4202014332567));
#21182=CARTESIAN_POINT('Origin',(9.39692620785909,-0.8,18.4202014332567));
#21183=CARTESIAN_POINT('Origin',(9.39692620785909,-0.8,18.4202014332567));
#21184=CARTESIAN_POINT('',(7.19692620785909,-0.5,18.4202014332567));
#21185=CARTESIAN_POINT('Origin',(9.39692620785909,-0.5,18.4202014332567));
#21186=CARTESIAN_POINT('',(7.19692620785909,-0.8,18.4202014332567));
#21187=CARTESIAN_POINT('',(7.19692620785909,-0.8,18.4202014332567));
#21188=CARTESIAN_POINT('Origin',(9.39692620785909,-0.8,18.4202014332567));
#21189=CARTESIAN_POINT('Origin',(9.39692620785909,-0.5,18.4202014332567));
#21190=CARTESIAN_POINT('Origin',(9.39692620785909,-0.8,18.4202014332567));
#21191=CARTESIAN_POINT('',(0.,0.,0.));
#21192=CARTESIAN_POINT('Origin',(10.7050737530542,-0.8,19.7283489784518));
#21193=CARTESIAN_POINT('',(10.3550737530542,-0.8,19.7283489784518));
#21194=CARTESIAN_POINT('Origin',(10.7050737530542,-0.8,19.7283489784518));
#21195=CARTESIAN_POINT('',(10.5050737530542,-0.8,19.7283489784518));
#21196=CARTESIAN_POINT('Origin',(10.7050737530542,-0.8,19.7283489784518));
#21197=CARTESIAN_POINT('Origin',(10.7050737530542,-1.2,19.7283489784518));
#21198=CARTESIAN_POINT('',(10.3550737530542,-1.2,19.7283489784518));
#21199=CARTESIAN_POINT('',(10.3550737530542,-1.2,19.7283489784518));
#21200=CARTESIAN_POINT('Origin',(10.7050737530542,-1.2,19.7283489784518));
#21201=CARTESIAN_POINT('Origin',(10.7050737530542,-1.2,19.7283489784518));
#21202=CARTESIAN_POINT('Origin',(10.7050737530542,-0.8,19.7283489784518));
#21203=CARTESIAN_POINT('',(10.5050737530542,-0.1,19.7283489784518));
#21204=CARTESIAN_POINT('Origin',(10.7050737530542,-0.1,19.7283489784518));
#21205=CARTESIAN_POINT('',(10.5050737530542,-0.8,19.7283489784518));
#21206=CARTESIAN_POINT('Origin',(10.7050737530542,-0.1,19.7283489784518));
#21207=CARTESIAN_POINT('',(0.,0.,0.));
#21208=CARTESIAN_POINT('Origin',(8.08877866266397,-0.8,19.7283489784518));
#21209=CARTESIAN_POINT('',(7.73877866266397,-0.8,19.7283489784518));
#21210=CARTESIAN_POINT('Origin',(8.08877866266397,-0.8,19.7283489784518));
#21211=CARTESIAN_POINT('',(7.88877866266397,-0.8,19.7283489784518));
#21212=CARTESIAN_POINT('Origin',(8.08877866266397,-0.8,19.7283489784518));
#21213=CARTESIAN_POINT('Origin',(8.08877866266397,-1.2,19.7283489784518));
#21214=CARTESIAN_POINT('',(7.73877866266397,-1.2,19.7283489784518));
#21215=CARTESIAN_POINT('',(7.73877866266397,-1.2,19.7283489784518));
#21216=CARTESIAN_POINT('Origin',(8.08877866266397,-1.2,19.7283489784518));
#21217=CARTESIAN_POINT('Origin',(8.08877866266397,-1.2,19.7283489784518));
#21218=CARTESIAN_POINT('Origin',(8.08877866266397,-0.8,19.7283489784518));
#21219=CARTESIAN_POINT('',(7.88877866266397,-0.1,19.7283489784518));
#21220=CARTESIAN_POINT('Origin',(8.08877866266397,-0.1,19.7283489784518));
#21221=CARTESIAN_POINT('',(7.88877866266397,-0.8,19.7283489784518));
#21222=CARTESIAN_POINT('Origin',(8.08877866266397,-0.1,19.7283489784518));
#21223=CARTESIAN_POINT('',(0.,0.,0.));
#21224=CARTESIAN_POINT('Origin',(8.08877866266397,-0.8,17.1120538880616));
#21225=CARTESIAN_POINT('',(7.73877866266397,-0.8,17.1120538880616));
#21226=CARTESIAN_POINT('Origin',(8.08877866266397,-0.8,17.1120538880616));
#21227=CARTESIAN_POINT('',(7.88877866266397,-0.8,17.1120538880616));
#21228=CARTESIAN_POINT('Origin',(8.08877866266397,-0.8,17.1120538880616));
#21229=CARTESIAN_POINT('Origin',(8.08877866266397,-1.2,17.1120538880616));
#21230=CARTESIAN_POINT('',(7.73877866266397,-1.2,17.1120538880616));
#21231=CARTESIAN_POINT('',(7.73877866266397,-1.2,17.1120538880616));
#21232=CARTESIAN_POINT('Origin',(8.08877866266397,-1.2,17.1120538880616));
#21233=CARTESIAN_POINT('Origin',(8.08877866266397,-1.2,17.1120538880616));
#21234=CARTESIAN_POINT('Origin',(8.08877866266397,-0.8,17.1120538880616));
#21235=CARTESIAN_POINT('',(7.88877866266397,-0.1,17.1120538880616));
#21236=CARTESIAN_POINT('Origin',(8.08877866266397,-0.1,17.1120538880616));
#21237=CARTESIAN_POINT('',(7.88877866266397,-0.8,17.1120538880616));
#21238=CARTESIAN_POINT('Origin',(8.08877866266397,-0.1,17.1120538880616));
#21239=CARTESIAN_POINT('',(0.,0.,0.));
#21240=CARTESIAN_POINT('Origin',(10.7050737530542,-0.8,17.1120538880616));
#21241=CARTESIAN_POINT('',(10.3550737530542,-0.8,17.1120538880616));
#21242=CARTESIAN_POINT('Origin',(10.7050737530542,-0.8,17.1120538880616));
#21243=CARTESIAN_POINT('',(10.5050737530542,-0.8,17.1120538880616));
#21244=CARTESIAN_POINT('Origin',(10.7050737530542,-0.8,17.1120538880616));
#21245=CARTESIAN_POINT('Origin',(10.7050737530542,-1.2,17.1120538880616));
#21246=CARTESIAN_POINT('',(10.3550737530542,-1.2,17.1120538880616));
#21247=CARTESIAN_POINT('',(10.3550737530542,-1.2,17.1120538880616));
#21248=CARTESIAN_POINT('Origin',(10.7050737530542,-1.2,17.1120538880616));
#21249=CARTESIAN_POINT('Origin',(10.7050737530542,-1.2,17.1120538880616));
#21250=CARTESIAN_POINT('Origin',(10.7050737530542,-0.8,17.1120538880616));
#21251=CARTESIAN_POINT('',(10.5050737530542,-0.1,17.1120538880616));
#21252=CARTESIAN_POINT('Origin',(10.7050737530542,-0.1,17.1120538880616));
#21253=CARTESIAN_POINT('',(10.5050737530542,-0.8,17.1120538880616));
#21254=CARTESIAN_POINT('Origin',(10.7050737530542,-0.1,17.1120538880616));
#21255=CARTESIAN_POINT('',(0.,0.,0.));
#21256=CARTESIAN_POINT('Origin',(8.08877866266397,0.4,17.1120538880616));
#21257=CARTESIAN_POINT('',(7.86377866266397,0.5,17.1120538880616));
#21258=CARTESIAN_POINT('Origin',(8.08877866266397,0.5,17.1120538880616));
#21259=CARTESIAN_POINT('',(7.86377866266397,0.8,17.1120538880616));
#21260=CARTESIAN_POINT('',(7.86377866266397,0.4,17.1120538880616));
#21261=CARTESIAN_POINT('Origin',(8.08877866266397,0.8,17.1120538880616));
#21262=CARTESIAN_POINT('Origin',(8.08877866266397,0.4,19.7283489784518));
#21263=CARTESIAN_POINT('',(7.86377866266397,0.5,19.7283489784518));
#21264=CARTESIAN_POINT('Origin',(8.08877866266397,0.5,19.7283489784518));
#21265=CARTESIAN_POINT('',(7.86377866266397,0.8,19.7283489784518));
#21266=CARTESIAN_POINT('',(7.86377866266397,0.4,19.7283489784518));
#21267=CARTESIAN_POINT('Origin',(8.08877866266397,0.8,19.7283489784518));
#21268=CARTESIAN_POINT('Origin',(10.7050737530542,0.4,19.7283489784518));
#21269=CARTESIAN_POINT('',(10.4800737530542,0.5,19.7283489784518));
#21270=CARTESIAN_POINT('Origin',(10.7050737530542,0.5,19.7283489784518));
#21271=CARTESIAN_POINT('',(10.4800737530542,0.8,19.7283489784518));
#21272=CARTESIAN_POINT('',(10.4800737530542,0.4,19.7283489784518));
#21273=CARTESIAN_POINT('Origin',(10.7050737530542,0.8,19.7283489784518));
#21274=CARTESIAN_POINT('Origin',(10.7050737530542,0.4,17.1120538880616));
#21275=CARTESIAN_POINT('',(10.4800737530542,0.5,17.1120538880616));
#21276=CARTESIAN_POINT('Origin',(10.7050737530542,0.5,17.1120538880616));
#21277=CARTESIAN_POINT('',(10.4800737530542,0.8,17.1120538880616));
#21278=CARTESIAN_POINT('',(10.4800737530542,0.4,17.1120538880616));
#21279=CARTESIAN_POINT('Origin',(10.7050737530542,0.8,17.1120538880616));
#21280=CARTESIAN_POINT('Origin',(9.39692620785909,0.5,18.4202014332567));
#21281=CARTESIAN_POINT('',(8.37692620785909,0.8,18.4202014332567));
#21282=CARTESIAN_POINT('Origin',(9.39692620785909,0.8,18.4202014332567));
#21283=CARTESIAN_POINT('',(8.37692620785909,0.5,18.4202014332567));
#21284=CARTESIAN_POINT('',(8.37692620785909,0.5,18.4202014332567));
#21285=CARTESIAN_POINT('Origin',(9.39692620785909,0.5,18.4202014332567));
#21286=CARTESIAN_POINT('Origin',(9.39692620785909,0.5,18.4202014332567));
#21287=CARTESIAN_POINT('',(7.19692620785909,0.8,18.4202014332567));
#21288=CARTESIAN_POINT('Origin',(9.39692620785909,0.8,18.4202014332567));
#21289=CARTESIAN_POINT('',(7.19692620785909,0.5,18.4202014332567));
#21290=CARTESIAN_POINT('',(7.19692620785909,0.5,18.4202014332567));
#21291=CARTESIAN_POINT('Origin',(9.39692620785909,0.5,18.4202014332567));
#21292=CARTESIAN_POINT('Origin',(9.39692620785909,0.8,18.4202014332567));
#21293=CARTESIAN_POINT('Origin',(9.39692620785909,0.5,18.4202014332567));
#21294=CARTESIAN_POINT('',(0.,0.,0.));
#21295=CARTESIAN_POINT('Origin',(10.7050737530542,0.8,19.7283489784518));
#21296=CARTESIAN_POINT('',(10.3550737530542,0.8,19.7283489784518));
#21297=CARTESIAN_POINT('Origin',(10.7050737530542,0.8,19.7283489784518));
#21298=CARTESIAN_POINT('',(10.5050737530542,0.8,19.7283489784518));
#21299=CARTESIAN_POINT('Origin',(10.7050737530542,0.8,19.7283489784518));
#21300=CARTESIAN_POINT('Origin',(10.7050737530542,0.8,19.7283489784518));
#21301=CARTESIAN_POINT('',(10.3550737530542,1.2,19.7283489784518));
#21302=CARTESIAN_POINT('Origin',(10.7050737530542,1.2,19.7283489784518));
#21303=CARTESIAN_POINT('',(10.3550737530542,0.8,19.7283489784518));
#21304=CARTESIAN_POINT('Origin',(10.7050737530542,1.2,19.7283489784518));
#21305=CARTESIAN_POINT('Origin',(10.7050737530542,0.1,19.7283489784518));
#21306=CARTESIAN_POINT('',(10.5050737530542,0.1,19.7283489784518));
#21307=CARTESIAN_POINT('',(10.5050737530542,0.1,19.7283489784518));
#21308=CARTESIAN_POINT('Origin',(10.7050737530542,0.1,19.7283489784518));
#21309=CARTESIAN_POINT('Origin',(10.7050737530542,0.1,19.7283489784518));
#21310=CARTESIAN_POINT('',(0.,0.,0.));
#21311=CARTESIAN_POINT('Origin',(8.08877866266397,0.8,19.7283489784518));
#21312=CARTESIAN_POINT('',(7.73877866266397,0.8,19.7283489784518));
#21313=CARTESIAN_POINT('Origin',(8.08877866266397,0.8,19.7283489784518));
#21314=CARTESIAN_POINT('',(7.88877866266397,0.8,19.7283489784518));
#21315=CARTESIAN_POINT('Origin',(8.08877866266397,0.8,19.7283489784518));
#21316=CARTESIAN_POINT('Origin',(8.08877866266397,0.8,19.7283489784518));
#21317=CARTESIAN_POINT('',(7.73877866266397,1.2,19.7283489784518));
#21318=CARTESIAN_POINT('Origin',(8.08877866266397,1.2,19.7283489784518));
#21319=CARTESIAN_POINT('',(7.73877866266397,0.8,19.7283489784518));
#21320=CARTESIAN_POINT('Origin',(8.08877866266397,1.2,19.7283489784518));
#21321=CARTESIAN_POINT('Origin',(8.08877866266397,0.1,19.7283489784518));
#21322=CARTESIAN_POINT('',(7.88877866266397,0.1,19.7283489784518));
#21323=CARTESIAN_POINT('',(7.88877866266397,0.1,19.7283489784518));
#21324=CARTESIAN_POINT('Origin',(8.08877866266397,0.1,19.7283489784518));
#21325=CARTESIAN_POINT('Origin',(8.08877866266397,0.1,19.7283489784518));
#21326=CARTESIAN_POINT('',(0.,0.,0.));
#21327=CARTESIAN_POINT('Origin',(8.08877866266397,0.8,17.1120538880616));
#21328=CARTESIAN_POINT('',(7.73877866266397,0.8,17.1120538880616));
#21329=CARTESIAN_POINT('Origin',(8.08877866266397,0.8,17.1120538880616));
#21330=CARTESIAN_POINT('',(7.88877866266397,0.8,17.1120538880616));
#21331=CARTESIAN_POINT('Origin',(8.08877866266397,0.8,17.1120538880616));
#21332=CARTESIAN_POINT('Origin',(8.08877866266397,0.8,17.1120538880616));
#21333=CARTESIAN_POINT('',(7.73877866266397,1.2,17.1120538880616));
#21334=CARTESIAN_POINT('Origin',(8.08877866266397,1.2,17.1120538880616));
#21335=CARTESIAN_POINT('',(7.73877866266397,0.8,17.1120538880616));
#21336=CARTESIAN_POINT('Origin',(8.08877866266397,1.2,17.1120538880616));
#21337=CARTESIAN_POINT('Origin',(8.08877866266397,0.1,17.1120538880616));
#21338=CARTESIAN_POINT('',(7.88877866266397,0.1,17.1120538880616));
#21339=CARTESIAN_POINT('',(7.88877866266397,0.1,17.1120538880616));
#21340=CARTESIAN_POINT('Origin',(8.08877866266397,0.1,17.1120538880616));
#21341=CARTESIAN_POINT('Origin',(8.08877866266397,0.1,17.1120538880616));
#21342=CARTESIAN_POINT('',(0.,0.,0.));
#21343=CARTESIAN_POINT('Origin',(10.7050737530542,0.8,17.1120538880616));
#21344=CARTESIAN_POINT('',(10.3550737530542,0.8,17.1120538880616));
#21345=CARTESIAN_POINT('Origin',(10.7050737530542,0.8,17.1120538880616));
#21346=CARTESIAN_POINT('',(10.5050737530542,0.8,17.1120538880616));
#21347=CARTESIAN_POINT('Origin',(10.7050737530542,0.8,17.1120538880616));
#21348=CARTESIAN_POINT('Origin',(10.7050737530542,0.8,17.1120538880616));
#21349=CARTESIAN_POINT('',(10.3550737530542,1.2,17.1120538880616));
#21350=CARTESIAN_POINT('Origin',(10.7050737530542,1.2,17.1120538880616));
#21351=CARTESIAN_POINT('',(10.3550737530542,0.8,17.1120538880616));
#21352=CARTESIAN_POINT('Origin',(10.7050737530542,1.2,17.1120538880616));
#21353=CARTESIAN_POINT('Origin',(10.7050737530542,0.1,17.1120538880616));
#21354=CARTESIAN_POINT('',(10.5050737530542,0.1,17.1120538880616));
#21355=CARTESIAN_POINT('',(10.5050737530542,0.1,17.1120538880616));
#21356=CARTESIAN_POINT('Origin',(10.7050737530542,0.1,17.1120538880616));
#21357=CARTESIAN_POINT('Origin',(10.7050737530542,0.1,17.1120538880616));
#21358=CARTESIAN_POINT('',(0.,0.,0.));
#21359=CARTESIAN_POINT('',(0.,0.,0.));
#21360=CARTESIAN_POINT('Origin',(22.893930933827,-0.6,27.3496056572921));
#21361=CARTESIAN_POINT('',(22.728930933827,-0.5,27.3496056572921));
#21362=CARTESIAN_POINT('Origin',(22.893930933827,-0.5,27.3496056572921));
#21363=CARTESIAN_POINT('',(22.728930933827,0.5,27.3496056572921));
#21364=CARTESIAN_POINT('',(22.728930933827,-0.6,27.3496056572921));
#21365=CARTESIAN_POINT('Origin',(22.893930933827,0.5,27.3496056572921));
#21366=CARTESIAN_POINT('Origin',(22.893930933827,-0.6,29.9659007476824));
#21367=CARTESIAN_POINT('',(22.728930933827,-0.5,29.9659007476824));
#21368=CARTESIAN_POINT('Origin',(22.893930933827,-0.5,29.9659007476824));
#21369=CARTESIAN_POINT('',(22.728930933827,0.5,29.9659007476824));
#21370=CARTESIAN_POINT('',(22.728930933827,-0.6,29.9659007476824));
#21371=CARTESIAN_POINT('Origin',(22.893930933827,0.5,29.9659007476824));
#21372=CARTESIAN_POINT('Origin',(25.5102260242172,-0.6,29.9659007476824));
#21373=CARTESIAN_POINT('',(25.3452260242172,-0.5,29.9659007476824));
#21374=CARTESIAN_POINT('Origin',(25.5102260242172,-0.5,29.9659007476824));
#21375=CARTESIAN_POINT('',(25.3452260242172,0.5,29.9659007476824));
#21376=CARTESIAN_POINT('',(25.3452260242172,-0.6,29.9659007476824));
#21377=CARTESIAN_POINT('Origin',(25.5102260242172,0.5,29.9659007476824));
#21378=CARTESIAN_POINT('Origin',(25.5102260242172,-0.6,27.3496056572921));
#21379=CARTESIAN_POINT('',(25.3452260242172,-0.5,27.3496056572921));
#21380=CARTESIAN_POINT('Origin',(25.5102260242172,-0.5,27.3496056572921));
#21381=CARTESIAN_POINT('',(25.3452260242172,0.5,27.3496056572921));
#21382=CARTESIAN_POINT('',(25.3452260242172,-0.6,27.3496056572921));
#21383=CARTESIAN_POINT('Origin',(25.5102260242172,0.5,27.3496056572921));
#21384=CARTESIAN_POINT('Origin',(24.2020784790221,-0.6,28.6577532024872));
#21385=CARTESIAN_POINT('',(22.6020784790221,-0.5,28.6577532024872));
#21386=CARTESIAN_POINT('Origin',(24.2020784790221,-0.5,28.6577532024872));
#21387=CARTESIAN_POINT('',(22.6020784790221,0.5,28.6577532024872));
#21388=CARTESIAN_POINT('',(22.6020784790221,-0.6,28.6577532024872));
#21389=CARTESIAN_POINT('Origin',(24.2020784790221,0.5,28.6577532024872));
#21390=CARTESIAN_POINT('Origin',(24.2020784790221,-0.5,28.6577532024872));
#21391=CARTESIAN_POINT('',(22.5525742431765,-0.5,27.2020280306477));
#21392=CARTESIAN_POINT('',(22.5525742431765,0.5,27.2020280306477));
#21393=CARTESIAN_POINT('',(22.5525742431765,-0.5,27.2020280306477));
#21394=CARTESIAN_POINT('',(24.191504627475,-0.5,26.457778613165));
#21395=CARTESIAN_POINT('Origin',(24.2020784790221,-0.5,28.6577532024872));
#21396=CARTESIAN_POINT('',(24.191504627475,0.5,26.457778613165));
#21397=CARTESIAN_POINT('',(24.191504627475,-0.5,26.457778613165));
#21398=CARTESIAN_POINT('Origin',(24.2020784790221,0.5,28.6577532024872));
#21399=CARTESIAN_POINT('Origin',(17.1805348078508,-0.5,15.3721247087413));
#21400=CARTESIAN_POINT('',(18.0105738515472,0.5,17.1999745893222));
#21401=CARTESIAN_POINT('',(17.1805348078508,0.5,15.3721247087413));
#21402=CARTESIAN_POINT('',(18.0105738515472,-0.5,17.1999745893222));
#21403=CARTESIAN_POINT('',(18.0105738515472,-0.5,17.1999745893222));
#21404=CARTESIAN_POINT('',(17.1805348078508,-0.5,15.3721247087413));
#21405=CARTESIAN_POINT('Origin',(21.1010392395111,0.5,21.8288766012436));
#21406=CARTESIAN_POINT('',(19.6495042358456,0.5,16.4557251718396));
#21407=CARTESIAN_POINT('',(25.0215436711714,0.5,28.2856284937459));
#21408=CARTESIAN_POINT('Origin',(18.,0.5,15.));
#21409=CARTESIAN_POINT('',(16.4,0.5,15.));
#21410=CARTESIAN_POINT('Origin',(18.,0.5,15.));
#21411=CARTESIAN_POINT('',(19.1431475451951,0.5,13.6918524548049));
#21412=CARTESIAN_POINT('Origin',(19.3081475451951,0.5,13.6918524548049));
#21413=CARTESIAN_POINT('',(19.1431475451951,0.5,16.3081475451951));
#21414=CARTESIAN_POINT('Origin',(19.3081475451951,0.5,16.3081475451951));
#21415=CARTESIAN_POINT('',(16.5268524548049,0.5,16.3081475451951));
#21416=CARTESIAN_POINT('Origin',(16.6918524548049,0.5,16.3081475451951));
#21417=CARTESIAN_POINT('',(16.5268524548049,0.5,13.6918524548049));
#21418=CARTESIAN_POINT('Origin',(16.6918524548049,0.5,13.6918524548049));
#21419=CARTESIAN_POINT('Origin',(16.6918524548049,-0.6,13.6918524548049));
#21420=CARTESIAN_POINT('',(16.5268524548049,-0.5,13.6918524548049));
#21421=CARTESIAN_POINT('Origin',(16.6918524548049,-0.5,13.6918524548049));
#21422=CARTESIAN_POINT('',(16.5268524548049,-0.6,13.6918524548049));
#21423=CARTESIAN_POINT('Origin',(16.6918524548049,-0.6,16.3081475451951));
#21424=CARTESIAN_POINT('',(16.5268524548049,-0.5,16.3081475451951));
#21425=CARTESIAN_POINT('Origin',(16.6918524548049,-0.5,16.3081475451951));
#21426=CARTESIAN_POINT('',(16.5268524548049,-0.6,16.3081475451951));
#21427=CARTESIAN_POINT('Origin',(19.3081475451951,-0.6,16.3081475451951));
#21428=CARTESIAN_POINT('',(19.1431475451951,-0.5,16.3081475451951));
#21429=CARTESIAN_POINT('Origin',(19.3081475451951,-0.5,16.3081475451951));
#21430=CARTESIAN_POINT('',(19.1431475451951,-0.6,16.3081475451951));
#21431=CARTESIAN_POINT('Origin',(19.3081475451951,-0.6,13.6918524548049));
#21432=CARTESIAN_POINT('',(19.1431475451951,-0.5,13.6918524548049));
#21433=CARTESIAN_POINT('Origin',(19.3081475451951,-0.5,13.6918524548049));
#21434=CARTESIAN_POINT('',(19.1431475451951,-0.6,13.6918524548049));
#21435=CARTESIAN_POINT('Origin',(18.,-0.6,15.));
#21436=CARTESIAN_POINT('',(16.4,-0.5,15.));
#21437=CARTESIAN_POINT('Origin',(18.,-0.5,15.));
#21438=CARTESIAN_POINT('',(16.4,-0.6,15.));
#21439=CARTESIAN_POINT('Origin',(18.,-0.5,15.));
#21440=CARTESIAN_POINT('',(19.6495042358456,-0.5,16.4557251718396));
#21441=CARTESIAN_POINT('',(19.6495042358456,-0.5,16.4557251718396));
#21442=CARTESIAN_POINT('Origin',(18.,-0.5,15.));
#21443=CARTESIAN_POINT('Origin',(25.0215436711714,-0.5,28.2856284937459));
#21444=CARTESIAN_POINT('',(25.0215436711714,-0.5,28.2856284937459));
#21445=CARTESIAN_POINT('Origin',(21.1010392395111,-0.5,21.8288766012436));
#21446=CARTESIAN_POINT('',(0.,0.,0.));
#21447=CARTESIAN_POINT('Origin',(16.6918524548049,-0.9,13.6918524548049));
#21448=CARTESIAN_POINT('',(16.4668524548049,-0.8,13.6918524548049));
#21449=CARTESIAN_POINT('Origin',(16.6918524548049,-0.8,13.6918524548049));
#21450=CARTESIAN_POINT('',(16.4668524548049,-0.5,13.6918524548049));
#21451=CARTESIAN_POINT('',(16.4668524548049,-0.9,13.6918524548049));
#21452=CARTESIAN_POINT('Origin',(16.6918524548049,-0.5,13.6918524548049));
#21453=CARTESIAN_POINT('Origin',(16.6918524548049,-0.9,16.3081475451951));
#21454=CARTESIAN_POINT('',(16.4668524548049,-0.8,16.3081475451951));
#21455=CARTESIAN_POINT('Origin',(16.6918524548049,-0.8,16.3081475451951));
#21456=CARTESIAN_POINT('',(16.4668524548049,-0.5,16.3081475451951));
#21457=CARTESIAN_POINT('',(16.4668524548049,-0.9,16.3081475451951));
#21458=CARTESIAN_POINT('Origin',(16.6918524548049,-0.5,16.3081475451951));
#21459=CARTESIAN_POINT('Origin',(19.3081475451951,-0.9,16.3081475451951));
#21460=CARTESIAN_POINT('',(19.0831475451951,-0.8,16.3081475451951));
#21461=CARTESIAN_POINT('Origin',(19.3081475451951,-0.8,16.3081475451951));
#21462=CARTESIAN_POINT('',(19.0831475451951,-0.5,16.3081475451951));
#21463=CARTESIAN_POINT('',(19.0831475451951,-0.9,16.3081475451951));
#21464=CARTESIAN_POINT('Origin',(19.3081475451951,-0.5,16.3081475451951));
#21465=CARTESIAN_POINT('Origin',(19.3081475451951,-0.9,13.6918524548049));
#21466=CARTESIAN_POINT('',(19.0831475451951,-0.8,13.6918524548049));
#21467=CARTESIAN_POINT('Origin',(19.3081475451951,-0.8,13.6918524548049));
#21468=CARTESIAN_POINT('',(19.0831475451951,-0.5,13.6918524548049));
#21469=CARTESIAN_POINT('',(19.0831475451951,-0.9,13.6918524548049));
#21470=CARTESIAN_POINT('Origin',(19.3081475451951,-0.5,13.6918524548049));
#21471=CARTESIAN_POINT('Origin',(18.,-0.8,15.));
#21472=CARTESIAN_POINT('',(16.98,-0.5,15.));
#21473=CARTESIAN_POINT('Origin',(18.,-0.5,15.));
#21474=CARTESIAN_POINT('',(16.98,-0.8,15.));
#21475=CARTESIAN_POINT('',(16.98,-0.8,15.));
#21476=CARTESIAN_POINT('Origin',(18.,-0.8,15.));
#21477=CARTESIAN_POINT('Origin',(18.,-0.8,15.));
#21478=CARTESIAN_POINT('',(15.8,-0.5,15.));
#21479=CARTESIAN_POINT('Origin',(18.,-0.5,15.));
#21480=CARTESIAN_POINT('',(15.8,-0.8,15.));
#21481=CARTESIAN_POINT('',(15.8,-0.8,15.));
#21482=CARTESIAN_POINT('Origin',(18.,-0.8,15.));
#21483=CARTESIAN_POINT('Origin',(18.,-0.5,15.));
#21484=CARTESIAN_POINT('Origin',(18.,-0.8,15.));
#21485=CARTESIAN_POINT('',(0.,0.,0.));
#21486=CARTESIAN_POINT('Origin',(19.3081475451951,-0.8,16.3081475451951));
#21487=CARTESIAN_POINT('',(18.9581475451951,-0.8,16.3081475451951));
#21488=CARTESIAN_POINT('Origin',(19.3081475451951,-0.8,16.3081475451951));
#21489=CARTESIAN_POINT('',(19.1081475451951,-0.8,16.3081475451951));
#21490=CARTESIAN_POINT('Origin',(19.3081475451951,-0.8,16.3081475451951));
#21491=CARTESIAN_POINT('Origin',(19.3081475451951,-1.2,16.3081475451951));
#21492=CARTESIAN_POINT('',(18.9581475451951,-1.2,16.3081475451951));
#21493=CARTESIAN_POINT('',(18.9581475451951,-1.2,16.3081475451951));
#21494=CARTESIAN_POINT('Origin',(19.3081475451951,-1.2,16.3081475451951));
#21495=CARTESIAN_POINT('Origin',(19.3081475451951,-1.2,16.3081475451951));
#21496=CARTESIAN_POINT('Origin',(19.3081475451951,-0.8,16.3081475451951));
#21497=CARTESIAN_POINT('',(19.1081475451951,-0.1,16.3081475451951));
#21498=CARTESIAN_POINT('Origin',(19.3081475451951,-0.1,16.3081475451951));
#21499=CARTESIAN_POINT('',(19.1081475451951,-0.8,16.3081475451951));
#21500=CARTESIAN_POINT('Origin',(19.3081475451951,-0.1,16.3081475451951));
#21501=CARTESIAN_POINT('',(0.,0.,0.));
#21502=CARTESIAN_POINT('Origin',(16.6918524548049,-0.8,16.3081475451951));
#21503=CARTESIAN_POINT('',(16.3418524548049,-0.8,16.3081475451951));
#21504=CARTESIAN_POINT('Origin',(16.6918524548049,-0.8,16.3081475451951));
#21505=CARTESIAN_POINT('',(16.4918524548049,-0.8,16.3081475451951));
#21506=CARTESIAN_POINT('Origin',(16.6918524548049,-0.8,16.3081475451951));
#21507=CARTESIAN_POINT('Origin',(16.6918524548049,-1.2,16.3081475451951));
#21508=CARTESIAN_POINT('',(16.3418524548049,-1.2,16.3081475451951));
#21509=CARTESIAN_POINT('',(16.3418524548049,-1.2,16.3081475451951));
#21510=CARTESIAN_POINT('Origin',(16.6918524548049,-1.2,16.3081475451951));
#21511=CARTESIAN_POINT('Origin',(16.6918524548049,-1.2,16.3081475451951));
#21512=CARTESIAN_POINT('Origin',(16.6918524548049,-0.8,16.3081475451951));
#21513=CARTESIAN_POINT('',(16.4918524548049,-0.1,16.3081475451951));
#21514=CARTESIAN_POINT('Origin',(16.6918524548049,-0.1,16.3081475451951));
#21515=CARTESIAN_POINT('',(16.4918524548049,-0.8,16.3081475451951));
#21516=CARTESIAN_POINT('Origin',(16.6918524548049,-0.1,16.3081475451951));
#21517=CARTESIAN_POINT('',(0.,0.,0.));
#21518=CARTESIAN_POINT('Origin',(16.6918524548049,-0.8,13.6918524548049));
#21519=CARTESIAN_POINT('',(16.3418524548049,-0.8,13.6918524548049));
#21520=CARTESIAN_POINT('Origin',(16.6918524548049,-0.8,13.6918524548049));
#21521=CARTESIAN_POINT('',(16.4918524548049,-0.8,13.6918524548049));
#21522=CARTESIAN_POINT('Origin',(16.6918524548049,-0.8,13.6918524548049));
#21523=CARTESIAN_POINT('Origin',(16.6918524548049,-1.2,13.6918524548049));
#21524=CARTESIAN_POINT('',(16.3418524548049,-1.2,13.6918524548049));
#21525=CARTESIAN_POINT('',(16.3418524548049,-1.2,13.6918524548049));
#21526=CARTESIAN_POINT('Origin',(16.6918524548049,-1.2,13.6918524548049));
#21527=CARTESIAN_POINT('Origin',(16.6918524548049,-1.2,13.6918524548049));
#21528=CARTESIAN_POINT('Origin',(16.6918524548049,-0.8,13.6918524548049));
#21529=CARTESIAN_POINT('',(16.4918524548049,-0.1,13.6918524548049));
#21530=CARTESIAN_POINT('Origin',(16.6918524548049,-0.1,13.6918524548049));
#21531=CARTESIAN_POINT('',(16.4918524548049,-0.8,13.6918524548049));
#21532=CARTESIAN_POINT('Origin',(16.6918524548049,-0.1,13.6918524548049));
#21533=CARTESIAN_POINT('',(0.,0.,0.));
#21534=CARTESIAN_POINT('Origin',(19.3081475451951,-0.8,13.6918524548049));
#21535=CARTESIAN_POINT('',(18.9581475451951,-0.8,13.6918524548049));
#21536=CARTESIAN_POINT('Origin',(19.3081475451951,-0.8,13.6918524548049));
#21537=CARTESIAN_POINT('',(19.1081475451951,-0.8,13.6918524548049));
#21538=CARTESIAN_POINT('Origin',(19.3081475451951,-0.8,13.6918524548049));
#21539=CARTESIAN_POINT('Origin',(19.3081475451951,-1.2,13.6918524548049));
#21540=CARTESIAN_POINT('',(18.9581475451951,-1.2,13.6918524548049));
#21541=CARTESIAN_POINT('',(18.9581475451951,-1.2,13.6918524548049));
#21542=CARTESIAN_POINT('Origin',(19.3081475451951,-1.2,13.6918524548049));
#21543=CARTESIAN_POINT('Origin',(19.3081475451951,-1.2,13.6918524548049));
#21544=CARTESIAN_POINT('Origin',(19.3081475451951,-0.8,13.6918524548049));
#21545=CARTESIAN_POINT('',(19.1081475451951,-0.1,13.6918524548049));
#21546=CARTESIAN_POINT('Origin',(19.3081475451951,-0.1,13.6918524548049));
#21547=CARTESIAN_POINT('',(19.1081475451951,-0.8,13.6918524548049));
#21548=CARTESIAN_POINT('Origin',(19.3081475451951,-0.1,13.6918524548049));
#21549=CARTESIAN_POINT('',(0.,0.,0.));
#21550=CARTESIAN_POINT('Origin',(16.6918524548049,0.4,13.6918524548049));
#21551=CARTESIAN_POINT('',(16.4668524548049,0.5,13.6918524548049));
#21552=CARTESIAN_POINT('Origin',(16.6918524548049,0.5,13.6918524548049));
#21553=CARTESIAN_POINT('',(16.4668524548049,0.8,13.6918524548049));
#21554=CARTESIAN_POINT('',(16.4668524548049,0.4,13.6918524548049));
#21555=CARTESIAN_POINT('Origin',(16.6918524548049,0.8,13.6918524548049));
#21556=CARTESIAN_POINT('Origin',(16.6918524548049,0.4,16.3081475451951));
#21557=CARTESIAN_POINT('',(16.4668524548049,0.5,16.3081475451951));
#21558=CARTESIAN_POINT('Origin',(16.6918524548049,0.5,16.3081475451951));
#21559=CARTESIAN_POINT('',(16.4668524548049,0.8,16.3081475451951));
#21560=CARTESIAN_POINT('',(16.4668524548049,0.4,16.3081475451951));
#21561=CARTESIAN_POINT('Origin',(16.6918524548049,0.8,16.3081475451951));
#21562=CARTESIAN_POINT('Origin',(19.3081475451951,0.4,16.3081475451951));
#21563=CARTESIAN_POINT('',(19.0831475451951,0.5,16.3081475451951));
#21564=CARTESIAN_POINT('Origin',(19.3081475451951,0.5,16.3081475451951));
#21565=CARTESIAN_POINT('',(19.0831475451951,0.8,16.3081475451951));
#21566=CARTESIAN_POINT('',(19.0831475451951,0.4,16.3081475451951));
#21567=CARTESIAN_POINT('Origin',(19.3081475451951,0.8,16.3081475451951));
#21568=CARTESIAN_POINT('Origin',(19.3081475451951,0.4,13.6918524548049));
#21569=CARTESIAN_POINT('',(19.0831475451951,0.5,13.6918524548049));
#21570=CARTESIAN_POINT('Origin',(19.3081475451951,0.5,13.6918524548049));
#21571=CARTESIAN_POINT('',(19.0831475451951,0.8,13.6918524548049));
#21572=CARTESIAN_POINT('',(19.0831475451951,0.4,13.6918524548049));
#21573=CARTESIAN_POINT('Origin',(19.3081475451951,0.8,13.6918524548049));
#21574=CARTESIAN_POINT('Origin',(18.,0.5,15.));
#21575=CARTESIAN_POINT('',(16.98,0.8,15.));
#21576=CARTESIAN_POINT('Origin',(18.,0.8,15.));
#21577=CARTESIAN_POINT('',(16.98,0.5,15.));
#21578=CARTESIAN_POINT('',(16.98,0.5,15.));
#21579=CARTESIAN_POINT('Origin',(18.,0.5,15.));
#21580=CARTESIAN_POINT('Origin',(18.,0.5,15.));
#21581=CARTESIAN_POINT('',(15.8,0.8,15.));
#21582=CARTESIAN_POINT('Origin',(18.,0.8,15.));
#21583=CARTESIAN_POINT('',(15.8,0.5,15.));
#21584=CARTESIAN_POINT('',(15.8,0.5,15.));
#21585=CARTESIAN_POINT('Origin',(18.,0.5,15.));
#21586=CARTESIAN_POINT('Origin',(18.,0.8,15.));
#21587=CARTESIAN_POINT('Origin',(18.,0.5,15.));
#21588=CARTESIAN_POINT('',(0.,0.,0.));
#21589=CARTESIAN_POINT('Origin',(19.3081475451951,0.8,16.3081475451951));
#21590=CARTESIAN_POINT('',(18.9581475451951,0.8,16.3081475451951));
#21591=CARTESIAN_POINT('Origin',(19.3081475451951,0.8,16.3081475451951));
#21592=CARTESIAN_POINT('',(19.1081475451951,0.8,16.3081475451951));
#21593=CARTESIAN_POINT('Origin',(19.3081475451951,0.8,16.3081475451951));
#21594=CARTESIAN_POINT('Origin',(19.3081475451951,0.8,16.3081475451951));
#21595=CARTESIAN_POINT('',(18.9581475451951,1.2,16.3081475451951));
#21596=CARTESIAN_POINT('Origin',(19.3081475451951,1.2,16.3081475451951));
#21597=CARTESIAN_POINT('',(18.9581475451951,0.8,16.3081475451951));
#21598=CARTESIAN_POINT('Origin',(19.3081475451951,1.2,16.3081475451951));
#21599=CARTESIAN_POINT('Origin',(19.3081475451951,0.1,16.3081475451951));
#21600=CARTESIAN_POINT('',(19.1081475451951,0.1,16.3081475451951));
#21601=CARTESIAN_POINT('',(19.1081475451951,0.1,16.3081475451951));
#21602=CARTESIAN_POINT('Origin',(19.3081475451951,0.1,16.3081475451951));
#21603=CARTESIAN_POINT('Origin',(19.3081475451951,0.1,16.3081475451951));
#21604=CARTESIAN_POINT('',(0.,0.,0.));
#21605=CARTESIAN_POINT('Origin',(16.6918524548049,0.8,16.3081475451951));
#21606=CARTESIAN_POINT('',(16.3418524548049,0.8,16.3081475451951));
#21607=CARTESIAN_POINT('Origin',(16.6918524548049,0.8,16.3081475451951));
#21608=CARTESIAN_POINT('',(16.4918524548049,0.8,16.3081475451951));
#21609=CARTESIAN_POINT('Origin',(16.6918524548049,0.8,16.3081475451951));
#21610=CARTESIAN_POINT('Origin',(16.6918524548049,0.8,16.3081475451951));
#21611=CARTESIAN_POINT('',(16.3418524548049,1.2,16.3081475451951));
#21612=CARTESIAN_POINT('Origin',(16.6918524548049,1.2,16.3081475451951));
#21613=CARTESIAN_POINT('',(16.3418524548049,0.8,16.3081475451951));
#21614=CARTESIAN_POINT('Origin',(16.6918524548049,1.2,16.3081475451951));
#21615=CARTESIAN_POINT('Origin',(16.6918524548049,0.1,16.3081475451951));
#21616=CARTESIAN_POINT('',(16.4918524548049,0.1,16.3081475451951));
#21617=CARTESIAN_POINT('',(16.4918524548049,0.1,16.3081475451951));
#21618=CARTESIAN_POINT('Origin',(16.6918524548049,0.1,16.3081475451951));
#21619=CARTESIAN_POINT('Origin',(16.6918524548049,0.1,16.3081475451951));
#21620=CARTESIAN_POINT('',(0.,0.,0.));
#21621=CARTESIAN_POINT('Origin',(16.6918524548049,0.8,13.6918524548049));
#21622=CARTESIAN_POINT('',(16.3418524548049,0.8,13.6918524548049));
#21623=CARTESIAN_POINT('Origin',(16.6918524548049,0.8,13.6918524548049));
#21624=CARTESIAN_POINT('',(16.4918524548049,0.8,13.6918524548049));
#21625=CARTESIAN_POINT('Origin',(16.6918524548049,0.8,13.6918524548049));
#21626=CARTESIAN_POINT('Origin',(16.6918524548049,0.8,13.6918524548049));
#21627=CARTESIAN_POINT('',(16.3418524548049,1.2,13.6918524548049));
#21628=CARTESIAN_POINT('Origin',(16.6918524548049,1.2,13.6918524548049));
#21629=CARTESIAN_POINT('',(16.3418524548049,0.8,13.6918524548049));
#21630=CARTESIAN_POINT('Origin',(16.6918524548049,1.2,13.6918524548049));
#21631=CARTESIAN_POINT('Origin',(16.6918524548049,0.1,13.6918524548049));
#21632=CARTESIAN_POINT('',(16.4918524548049,0.1,13.6918524548049));
#21633=CARTESIAN_POINT('',(16.4918524548049,0.1,13.6918524548049));
#21634=CARTESIAN_POINT('Origin',(16.6918524548049,0.1,13.6918524548049));
#21635=CARTESIAN_POINT('Origin',(16.6918524548049,0.1,13.6918524548049));
#21636=CARTESIAN_POINT('',(0.,0.,0.));
#21637=CARTESIAN_POINT('Origin',(19.3081475451951,0.8,13.6918524548049));
#21638=CARTESIAN_POINT('',(18.9581475451951,0.8,13.6918524548049));
#21639=CARTESIAN_POINT('Origin',(19.3081475451951,0.8,13.6918524548049));
#21640=CARTESIAN_POINT('',(19.1081475451951,0.8,13.6918524548049));
#21641=CARTESIAN_POINT('Origin',(19.3081475451951,0.8,13.6918524548049));
#21642=CARTESIAN_POINT('Origin',(19.3081475451951,0.8,13.6918524548049));
#21643=CARTESIAN_POINT('',(18.9581475451951,1.2,13.6918524548049));
#21644=CARTESIAN_POINT('Origin',(19.3081475451951,1.2,13.6918524548049));
#21645=CARTESIAN_POINT('',(18.9581475451951,0.8,13.6918524548049));
#21646=CARTESIAN_POINT('Origin',(19.3081475451951,1.2,13.6918524548049));
#21647=CARTESIAN_POINT('Origin',(19.3081475451951,0.1,13.6918524548049));
#21648=CARTESIAN_POINT('',(19.1081475451951,0.1,13.6918524548049));
#21649=CARTESIAN_POINT('',(19.1081475451951,0.1,13.6918524548049));
#21650=CARTESIAN_POINT('Origin',(19.3081475451951,0.1,13.6918524548049));
#21651=CARTESIAN_POINT('Origin',(19.3081475451951,0.1,13.6918524548049));
#21652=CARTESIAN_POINT('',(0.,0.,0.));
#21653=CARTESIAN_POINT('Origin',(22.893930933827,-0.9,27.3496056572921));
#21654=CARTESIAN_POINT('',(22.668930933827,-0.8,27.3496056572921));
#21655=CARTESIAN_POINT('Origin',(22.893930933827,-0.8,27.3496056572921));
#21656=CARTESIAN_POINT('',(22.668930933827,-0.5,27.3496056572921));
#21657=CARTESIAN_POINT('',(22.668930933827,-0.9,27.3496056572921));
#21658=CARTESIAN_POINT('Origin',(22.893930933827,-0.5,27.3496056572921));
#21659=CARTESIAN_POINT('Origin',(22.893930933827,-0.9,29.9659007476824));
#21660=CARTESIAN_POINT('',(22.668930933827,-0.8,29.9659007476824));
#21661=CARTESIAN_POINT('Origin',(22.893930933827,-0.8,29.9659007476824));
#21662=CARTESIAN_POINT('',(22.668930933827,-0.5,29.9659007476824));
#21663=CARTESIAN_POINT('',(22.668930933827,-0.9,29.9659007476824));
#21664=CARTESIAN_POINT('Origin',(22.893930933827,-0.5,29.9659007476824));
#21665=CARTESIAN_POINT('Origin',(25.5102260242172,-0.9,29.9659007476824));
#21666=CARTESIAN_POINT('',(25.2852260242172,-0.8,29.9659007476824));
#21667=CARTESIAN_POINT('Origin',(25.5102260242172,-0.8,29.9659007476824));
#21668=CARTESIAN_POINT('',(25.2852260242172,-0.5,29.9659007476824));
#21669=CARTESIAN_POINT('',(25.2852260242172,-0.9,29.9659007476824));
#21670=CARTESIAN_POINT('Origin',(25.5102260242172,-0.5,29.9659007476824));
#21671=CARTESIAN_POINT('Origin',(25.5102260242172,-0.9,27.3496056572921));
#21672=CARTESIAN_POINT('',(25.2852260242172,-0.8,27.3496056572921));
#21673=CARTESIAN_POINT('Origin',(25.5102260242172,-0.8,27.3496056572921));
#21674=CARTESIAN_POINT('',(25.2852260242172,-0.5,27.3496056572921));
#21675=CARTESIAN_POINT('',(25.2852260242172,-0.9,27.3496056572921));
#21676=CARTESIAN_POINT('Origin',(25.5102260242172,-0.5,27.3496056572921));
#21677=CARTESIAN_POINT('Origin',(24.2020784790221,-0.8,28.6577532024872));
#21678=CARTESIAN_POINT('',(23.1820784790221,-0.5,28.6577532024872));
#21679=CARTESIAN_POINT('Origin',(24.2020784790221,-0.5,28.6577532024872));
#21680=CARTESIAN_POINT('',(23.1820784790221,-0.8,28.6577532024872));
#21681=CARTESIAN_POINT('',(23.1820784790221,-0.8,28.6577532024872));
#21682=CARTESIAN_POINT('Origin',(24.2020784790221,-0.8,28.6577532024872));
#21683=CARTESIAN_POINT('Origin',(24.2020784790221,-0.8,28.6577532024872));
#21684=CARTESIAN_POINT('',(22.0020784790221,-0.5,28.6577532024872));
#21685=CARTESIAN_POINT('Origin',(24.2020784790221,-0.5,28.6577532024872));
#21686=CARTESIAN_POINT('',(22.0020784790221,-0.8,28.6577532024872));
#21687=CARTESIAN_POINT('',(22.0020784790221,-0.8,28.6577532024872));
#21688=CARTESIAN_POINT('Origin',(24.2020784790221,-0.8,28.6577532024872));
#21689=CARTESIAN_POINT('Origin',(24.2020784790221,-0.5,28.6577532024872));
#21690=CARTESIAN_POINT('Origin',(24.2020784790221,-0.8,28.6577532024872));
#21691=CARTESIAN_POINT('',(0.,0.,0.));
#21692=CARTESIAN_POINT('Origin',(25.5102260242172,-0.8,29.9659007476824));
#21693=CARTESIAN_POINT('',(25.1602260242172,-0.8,29.9659007476824));
#21694=CARTESIAN_POINT('Origin',(25.5102260242172,-0.8,29.9659007476824));
#21695=CARTESIAN_POINT('',(25.3102260242172,-0.8,29.9659007476824));
#21696=CARTESIAN_POINT('Origin',(25.5102260242172,-0.8,29.9659007476824));
#21697=CARTESIAN_POINT('Origin',(25.5102260242172,-1.2,29.9659007476824));
#21698=CARTESIAN_POINT('',(25.1602260242172,-1.2,29.9659007476824));
#21699=CARTESIAN_POINT('',(25.1602260242172,-1.2,29.9659007476824));
#21700=CARTESIAN_POINT('Origin',(25.5102260242172,-1.2,29.9659007476824));
#21701=CARTESIAN_POINT('Origin',(25.5102260242172,-1.2,29.9659007476824));
#21702=CARTESIAN_POINT('Origin',(25.5102260242172,-0.8,29.9659007476824));
#21703=CARTESIAN_POINT('',(25.3102260242172,-0.1,29.9659007476824));
#21704=CARTESIAN_POINT('Origin',(25.5102260242172,-0.1,29.9659007476824));
#21705=CARTESIAN_POINT('',(25.3102260242172,-0.8,29.9659007476824));
#21706=CARTESIAN_POINT('Origin',(25.5102260242172,-0.1,29.9659007476824));
#21707=CARTESIAN_POINT('',(0.,0.,0.));
#21708=CARTESIAN_POINT('Origin',(22.893930933827,-0.8,29.9659007476824));
#21709=CARTESIAN_POINT('',(22.543930933827,-0.8,29.9659007476824));
#21710=CARTESIAN_POINT('Origin',(22.893930933827,-0.8,29.9659007476824));
#21711=CARTESIAN_POINT('',(22.693930933827,-0.8,29.9659007476824));
#21712=CARTESIAN_POINT('Origin',(22.893930933827,-0.8,29.9659007476824));
#21713=CARTESIAN_POINT('Origin',(22.893930933827,-1.2,29.9659007476824));
#21714=CARTESIAN_POINT('',(22.543930933827,-1.2,29.9659007476824));
#21715=CARTESIAN_POINT('',(22.543930933827,-1.2,29.9659007476824));
#21716=CARTESIAN_POINT('Origin',(22.893930933827,-1.2,29.9659007476824));
#21717=CARTESIAN_POINT('Origin',(22.893930933827,-1.2,29.9659007476824));
#21718=CARTESIAN_POINT('Origin',(22.893930933827,-0.8,29.9659007476824));
#21719=CARTESIAN_POINT('',(22.693930933827,-0.1,29.9659007476824));
#21720=CARTESIAN_POINT('Origin',(22.893930933827,-0.1,29.9659007476824));
#21721=CARTESIAN_POINT('',(22.693930933827,-0.8,29.9659007476824));
#21722=CARTESIAN_POINT('Origin',(22.893930933827,-0.1,29.9659007476824));
#21723=CARTESIAN_POINT('',(0.,0.,0.));
#21724=CARTESIAN_POINT('Origin',(22.893930933827,-0.8,27.3496056572921));
#21725=CARTESIAN_POINT('',(22.543930933827,-0.8,27.3496056572921));
#21726=CARTESIAN_POINT('Origin',(22.893930933827,-0.8,27.3496056572921));
#21727=CARTESIAN_POINT('',(22.693930933827,-0.8,27.3496056572921));
#21728=CARTESIAN_POINT('Origin',(22.893930933827,-0.8,27.3496056572921));
#21729=CARTESIAN_POINT('Origin',(22.893930933827,-1.2,27.3496056572921));
#21730=CARTESIAN_POINT('',(22.543930933827,-1.2,27.3496056572921));
#21731=CARTESIAN_POINT('',(22.543930933827,-1.2,27.3496056572921));
#21732=CARTESIAN_POINT('Origin',(22.893930933827,-1.2,27.3496056572921));
#21733=CARTESIAN_POINT('Origin',(22.893930933827,-1.2,27.3496056572921));
#21734=CARTESIAN_POINT('Origin',(22.893930933827,-0.8,27.3496056572921));
#21735=CARTESIAN_POINT('',(22.693930933827,-0.1,27.3496056572921));
#21736=CARTESIAN_POINT('Origin',(22.893930933827,-0.1,27.3496056572921));
#21737=CARTESIAN_POINT('',(22.693930933827,-0.8,27.3496056572921));
#21738=CARTESIAN_POINT('Origin',(22.893930933827,-0.1,27.3496056572921));
#21739=CARTESIAN_POINT('',(0.,0.,0.));
#21740=CARTESIAN_POINT('Origin',(25.5102260242172,-0.8,27.3496056572921));
#21741=CARTESIAN_POINT('',(25.1602260242172,-0.8,27.3496056572921));
#21742=CARTESIAN_POINT('Origin',(25.5102260242172,-0.8,27.3496056572921));
#21743=CARTESIAN_POINT('',(25.3102260242172,-0.8,27.3496056572921));
#21744=CARTESIAN_POINT('Origin',(25.5102260242172,-0.8,27.3496056572921));
#21745=CARTESIAN_POINT('Origin',(25.5102260242172,-1.2,27.3496056572921));
#21746=CARTESIAN_POINT('',(25.1602260242172,-1.2,27.3496056572921));
#21747=CARTESIAN_POINT('',(25.1602260242172,-1.2,27.3496056572921));
#21748=CARTESIAN_POINT('Origin',(25.5102260242172,-1.2,27.3496056572921));
#21749=CARTESIAN_POINT('Origin',(25.5102260242172,-1.2,27.3496056572921));
#21750=CARTESIAN_POINT('Origin',(25.5102260242172,-0.8,27.3496056572921));
#21751=CARTESIAN_POINT('',(25.3102260242172,-0.1,27.3496056572921));
#21752=CARTESIAN_POINT('Origin',(25.5102260242172,-0.1,27.3496056572921));
#21753=CARTESIAN_POINT('',(25.3102260242172,-0.8,27.3496056572921));
#21754=CARTESIAN_POINT('Origin',(25.5102260242172,-0.1,27.3496056572921));
#21755=CARTESIAN_POINT('',(0.,0.,0.));
#21756=CARTESIAN_POINT('Origin',(22.893930933827,0.4,27.3496056572921));
#21757=CARTESIAN_POINT('',(22.668930933827,0.5,27.3496056572921));
#21758=CARTESIAN_POINT('Origin',(22.893930933827,0.5,27.3496056572921));
#21759=CARTESIAN_POINT('',(22.668930933827,0.8,27.3496056572921));
#21760=CARTESIAN_POINT('',(22.668930933827,0.4,27.3496056572921));
#21761=CARTESIAN_POINT('Origin',(22.893930933827,0.8,27.3496056572921));
#21762=CARTESIAN_POINT('Origin',(22.893930933827,0.4,29.9659007476824));
#21763=CARTESIAN_POINT('',(22.668930933827,0.5,29.9659007476824));
#21764=CARTESIAN_POINT('Origin',(22.893930933827,0.5,29.9659007476824));
#21765=CARTESIAN_POINT('',(22.668930933827,0.8,29.9659007476824));
#21766=CARTESIAN_POINT('',(22.668930933827,0.4,29.9659007476824));
#21767=CARTESIAN_POINT('Origin',(22.893930933827,0.8,29.9659007476824));
#21768=CARTESIAN_POINT('Origin',(25.5102260242172,0.4,29.9659007476824));
#21769=CARTESIAN_POINT('',(25.2852260242172,0.5,29.9659007476824));
#21770=CARTESIAN_POINT('Origin',(25.5102260242172,0.5,29.9659007476824));
#21771=CARTESIAN_POINT('',(25.2852260242172,0.8,29.9659007476824));
#21772=CARTESIAN_POINT('',(25.2852260242172,0.4,29.9659007476824));
#21773=CARTESIAN_POINT('Origin',(25.5102260242172,0.8,29.9659007476824));
#21774=CARTESIAN_POINT('Origin',(25.5102260242172,0.4,27.3496056572921));
#21775=CARTESIAN_POINT('',(25.2852260242172,0.5,27.3496056572921));
#21776=CARTESIAN_POINT('Origin',(25.5102260242172,0.5,27.3496056572921));
#21777=CARTESIAN_POINT('',(25.2852260242172,0.8,27.3496056572921));
#21778=CARTESIAN_POINT('',(25.2852260242172,0.4,27.3496056572921));
#21779=CARTESIAN_POINT('Origin',(25.5102260242172,0.8,27.3496056572921));
#21780=CARTESIAN_POINT('Origin',(24.2020784790221,0.5,28.6577532024872));
#21781=CARTESIAN_POINT('',(23.1820784790221,0.8,28.6577532024872));
#21782=CARTESIAN_POINT('Origin',(24.2020784790221,0.8,28.6577532024872));
#21783=CARTESIAN_POINT('',(23.1820784790221,0.5,28.6577532024872));
#21784=CARTESIAN_POINT('',(23.1820784790221,0.5,28.6577532024872));
#21785=CARTESIAN_POINT('Origin',(24.2020784790221,0.5,28.6577532024872));
#21786=CARTESIAN_POINT('Origin',(24.2020784790221,0.5,28.6577532024872));
#21787=CARTESIAN_POINT('',(22.0020784790221,0.8,28.6577532024872));
#21788=CARTESIAN_POINT('Origin',(24.2020784790221,0.8,28.6577532024872));
#21789=CARTESIAN_POINT('',(22.0020784790221,0.5,28.6577532024872));
#21790=CARTESIAN_POINT('',(22.0020784790221,0.5,28.6577532024872));
#21791=CARTESIAN_POINT('Origin',(24.2020784790221,0.5,28.6577532024872));
#21792=CARTESIAN_POINT('Origin',(24.2020784790221,0.8,28.6577532024872));
#21793=CARTESIAN_POINT('Origin',(24.2020784790221,0.5,28.6577532024872));
#21794=CARTESIAN_POINT('',(0.,0.,0.));
#21795=CARTESIAN_POINT('Origin',(25.5102260242172,0.8,29.9659007476824));
#21796=CARTESIAN_POINT('',(25.1602260242172,0.8,29.9659007476824));
#21797=CARTESIAN_POINT('Origin',(25.5102260242172,0.8,29.9659007476824));
#21798=CARTESIAN_POINT('',(25.3102260242172,0.8,29.9659007476824));
#21799=CARTESIAN_POINT('Origin',(25.5102260242172,0.8,29.9659007476824));
#21800=CARTESIAN_POINT('Origin',(25.5102260242172,0.8,29.9659007476824));
#21801=CARTESIAN_POINT('',(25.1602260242172,1.2,29.9659007476824));
#21802=CARTESIAN_POINT('Origin',(25.5102260242172,1.2,29.9659007476824));
#21803=CARTESIAN_POINT('',(25.1602260242172,0.8,29.9659007476824));
#21804=CARTESIAN_POINT('Origin',(25.5102260242172,1.2,29.9659007476824));
#21805=CARTESIAN_POINT('Origin',(25.5102260242172,0.1,29.9659007476824));
#21806=CARTESIAN_POINT('',(25.3102260242172,0.1,29.9659007476824));
#21807=CARTESIAN_POINT('',(25.3102260242172,0.1,29.9659007476824));
#21808=CARTESIAN_POINT('Origin',(25.5102260242172,0.1,29.9659007476824));
#21809=CARTESIAN_POINT('Origin',(25.5102260242172,0.1,29.9659007476824));
#21810=CARTESIAN_POINT('',(0.,0.,0.));
#21811=CARTESIAN_POINT('Origin',(22.893930933827,0.8,29.9659007476824));
#21812=CARTESIAN_POINT('',(22.543930933827,0.8,29.9659007476824));
#21813=CARTESIAN_POINT('Origin',(22.893930933827,0.8,29.9659007476824));
#21814=CARTESIAN_POINT('',(22.693930933827,0.8,29.9659007476824));
#21815=CARTESIAN_POINT('Origin',(22.893930933827,0.8,29.9659007476824));
#21816=CARTESIAN_POINT('Origin',(22.893930933827,0.8,29.9659007476824));
#21817=CARTESIAN_POINT('',(22.543930933827,1.2,29.9659007476824));
#21818=CARTESIAN_POINT('Origin',(22.893930933827,1.2,29.9659007476824));
#21819=CARTESIAN_POINT('',(22.543930933827,0.8,29.9659007476824));
#21820=CARTESIAN_POINT('Origin',(22.893930933827,1.2,29.9659007476824));
#21821=CARTESIAN_POINT('Origin',(22.893930933827,0.1,29.9659007476824));
#21822=CARTESIAN_POINT('',(22.693930933827,0.1,29.9659007476824));
#21823=CARTESIAN_POINT('',(22.693930933827,0.1,29.9659007476824));
#21824=CARTESIAN_POINT('Origin',(22.893930933827,0.1,29.9659007476824));
#21825=CARTESIAN_POINT('Origin',(22.893930933827,0.1,29.9659007476824));
#21826=CARTESIAN_POINT('',(0.,0.,0.));
#21827=CARTESIAN_POINT('Origin',(22.893930933827,0.8,27.3496056572921));
#21828=CARTESIAN_POINT('',(22.543930933827,0.8,27.3496056572921));
#21829=CARTESIAN_POINT('Origin',(22.893930933827,0.8,27.3496056572921));
#21830=CARTESIAN_POINT('',(22.693930933827,0.8,27.3496056572921));
#21831=CARTESIAN_POINT('Origin',(22.893930933827,0.8,27.3496056572921));
#21832=CARTESIAN_POINT('Origin',(22.893930933827,0.8,27.3496056572921));
#21833=CARTESIAN_POINT('',(22.543930933827,1.2,27.3496056572921));
#21834=CARTESIAN_POINT('Origin',(22.893930933827,1.2,27.3496056572921));
#21835=CARTESIAN_POINT('',(22.543930933827,0.8,27.3496056572921));
#21836=CARTESIAN_POINT('Origin',(22.893930933827,1.2,27.3496056572921));
#21837=CARTESIAN_POINT('Origin',(22.893930933827,0.1,27.3496056572921));
#21838=CARTESIAN_POINT('',(22.693930933827,0.1,27.3496056572921));
#21839=CARTESIAN_POINT('',(22.693930933827,0.1,27.3496056572921));
#21840=CARTESIAN_POINT('Origin',(22.893930933827,0.1,27.3496056572921));
#21841=CARTESIAN_POINT('Origin',(22.893930933827,0.1,27.3496056572921));
#21842=CARTESIAN_POINT('',(0.,0.,0.));
#21843=CARTESIAN_POINT('Origin',(25.5102260242172,0.8,27.3496056572921));
#21844=CARTESIAN_POINT('',(25.1602260242172,0.8,27.3496056572921));
#21845=CARTESIAN_POINT('Origin',(25.5102260242172,0.8,27.3496056572921));
#21846=CARTESIAN_POINT('',(25.3102260242172,0.8,27.3496056572921));
#21847=CARTESIAN_POINT('Origin',(25.5102260242172,0.8,27.3496056572921));
#21848=CARTESIAN_POINT('Origin',(25.5102260242172,0.8,27.3496056572921));
#21849=CARTESIAN_POINT('',(25.1602260242172,1.2,27.3496056572921));
#21850=CARTESIAN_POINT('Origin',(25.5102260242172,1.2,27.3496056572921));
#21851=CARTESIAN_POINT('',(25.1602260242172,0.8,27.3496056572921));
#21852=CARTESIAN_POINT('Origin',(25.5102260242172,1.2,27.3496056572921));
#21853=CARTESIAN_POINT('Origin',(25.5102260242172,0.1,27.3496056572921));
#21854=CARTESIAN_POINT('',(25.3102260242172,0.1,27.3496056572921));
#21855=CARTESIAN_POINT('',(25.3102260242172,0.1,27.3496056572921));
#21856=CARTESIAN_POINT('Origin',(25.5102260242172,0.1,27.3496056572921));
#21857=CARTESIAN_POINT('Origin',(25.5102260242172,0.1,27.3496056572921));
#21858=CARTESIAN_POINT('',(0.,0.,0.));
#21859=CARTESIAN_POINT('',(0.,0.,0.));
#21860=CARTESIAN_POINT('Origin',(0.,0.,0.));
#21861=CARTESIAN_POINT('',(-1.070235,-0.308121667383195,-1.31065986708547E-16));
#21862=CARTESIAN_POINT('',(-1.31065986708547E-16,-0.308121667383195,1.070235));
#21863=CARTESIAN_POINT('Origin',(0.,-0.308121667383195,0.));
#21864=CARTESIAN_POINT('Origin',(0.,-0.308121667383195,0.));
#21865=CARTESIAN_POINT('',(-1.31065986708547E-16,0.308121667383195,1.070235));
#21866=CARTESIAN_POINT('Origin',(-1.34711147906209E-16,0.,1.1));
#21867=CARTESIAN_POINT('',(-1.070235,0.308121667383195,1.31065986708547E-16));
#21868=CARTESIAN_POINT('Origin',(0.,0.308121667383195,0.));
#21869=CARTESIAN_POINT('Origin',(0.,0.308121667383195,0.));
#21870=CARTESIAN_POINT('Origin',(0.,0.,0.));
#21871=CARTESIAN_POINT('',(-1.070235,0.5,-1.31065986708547E-16));
#21872=CARTESIAN_POINT('',(-1.070235,0.,-1.31065986708547E-16));
#21873=CARTESIAN_POINT('Origin',(0.,0.5,0.));
#21874=CARTESIAN_POINT('Origin',(0.,0.,0.));
#21875=CARTESIAN_POINT('',(-0.6,-0.44,-7.34788079488412E-17));
#21876=CARTESIAN_POINT('Origin',(0.,-0.44,0.));
#21877=CARTESIAN_POINT('',(-0.6,0.44,-7.34788079488412E-17));
#21878=CARTESIAN_POINT('',(-0.6,0.,-7.34788079488412E-17));
#21879=CARTESIAN_POINT('Origin',(0.,0.44,0.));
#21880=CARTESIAN_POINT('Origin',(0.,0.47,0.));
#21881=CARTESIAN_POINT('',(-0.66,0.5,-8.08266887437253E-17));
#21882=CARTESIAN_POINT('',(-0.63,0.47,-7.71527483462832E-17));
#21883=CARTESIAN_POINT('Origin',(0.,0.5,0.));
#21884=CARTESIAN_POINT('Origin',(1.070235,0.5,0.));
#21885=CARTESIAN_POINT('Origin',(0.,0.,0.));
#21886=CARTESIAN_POINT('',(-1.070235,-0.5,-1.31065986708547E-16));
#21887=CARTESIAN_POINT('Origin',(0.,-0.5,0.));
#21888=CARTESIAN_POINT('',(-1.070235,0.,-1.31065986708547E-16));
#21889=CARTESIAN_POINT('Origin',(0.66,-0.5,0.));
#21890=CARTESIAN_POINT('',(-0.66,-0.5,-8.08266887437253E-17));
#21891=CARTESIAN_POINT('Origin',(0.,-0.5,0.));
#21892=CARTESIAN_POINT('Origin',(0.,-0.47,0.));
#21893=CARTESIAN_POINT('',(-0.63,-0.47,-7.71527483462832E-17));
#21894=CARTESIAN_POINT('',(0.,0.,0.));
#21895=CARTESIAN_POINT('Origin',(0.,0.,0.));
#21896=CARTESIAN_POINT('',(-1.129765,0.308121667383195,-1.38356309103871E-16));
#21897=CARTESIAN_POINT('',(-1.38356309103871E-16,0.308121667383195,1.129765));
#21898=CARTESIAN_POINT('Origin',(0.,0.308121667383195,0.));
#21899=CARTESIAN_POINT('Origin',(0.,0.308121667383195,0.));
#21900=CARTESIAN_POINT('',(-1.38356309103871E-16,-0.308121667383195,1.129765));
#21901=CARTESIAN_POINT('Origin',(-1.34711147906209E-16,0.,1.1));
#21902=CARTESIAN_POINT('',(-1.129765,-0.308121667383195,1.38356309103871E-16));
#21903=CARTESIAN_POINT('Origin',(0.,-0.308121667383195,0.));
#21904=CARTESIAN_POINT('Origin',(0.,-0.308121667383195,0.));
#21905=CARTESIAN_POINT('Origin',(0.,0.,0.));
#21906=CARTESIAN_POINT('',(-1.129765,-0.5,-1.38356309103871E-16));
#21907=CARTESIAN_POINT('Origin',(0.,-0.5,0.));
#21908=CARTESIAN_POINT('',(-1.129765,0.,-1.38356309103871E-16));
#21909=CARTESIAN_POINT('Origin',(1.54,0.5,0.));
#21910=CARTESIAN_POINT('',(-1.54,0.5,-1.88595607068692E-16));
#21911=CARTESIAN_POINT('Origin',(0.,0.5,0.));
#21912=CARTESIAN_POINT('',(-1.129765,0.5,-1.38356309103871E-16));
#21913=CARTESIAN_POINT('Origin',(0.,0.5,0.));
#21914=CARTESIAN_POINT('Origin',(0.,0.47,0.));
#21915=CARTESIAN_POINT('',(-1.6,0.44,-1.95943487863577E-16));
#21916=CARTESIAN_POINT('Origin',(0.,0.44,0.));
#21917=CARTESIAN_POINT('',(-1.57,0.47,-1.92269547466134E-16));
#21918=CARTESIAN_POINT('Origin',(0.,0.,0.));
#21919=CARTESIAN_POINT('',(-1.6,-0.44,-1.95943487863577E-16));
#21920=CARTESIAN_POINT('Origin',(0.,-0.44,0.));
#21921=CARTESIAN_POINT('',(-1.6,0.,-1.95943487863577E-16));
#21922=CARTESIAN_POINT('Origin',(0.,-0.47,0.));
#21923=CARTESIAN_POINT('',(-1.54,-0.5,-1.88595607068692E-16));
#21924=CARTESIAN_POINT('Origin',(0.,-0.5,0.));
#21925=CARTESIAN_POINT('',(-1.57,-0.47,-1.92269547466134E-16));
#21926=CARTESIAN_POINT('Origin',(1.129765,-0.5,0.));
#21927=CARTESIAN_POINT('Origin',(0.,0.,0.));
#21928=CARTESIAN_POINT('',(-1.129765,0.,-1.38356309103871E-16));
#21929=CARTESIAN_POINT('',(0.,0.,0.));
#21930=CARTESIAN_POINT('Origin',(1.1,0.,0.));
#21931=CARTESIAN_POINT('',(1.1,-2.23201749654651E-33,0.29765));
#21932=CARTESIAN_POINT('',(1.1,-2.23201749654651E-33,-0.29765));
#21933=CARTESIAN_POINT('Origin',(1.1,0.,0.));
#21934=CARTESIAN_POINT('Origin',(0.685838782044607,0.,-0.860014630714833));
#21935=CARTESIAN_POINT('',(0.918550922801216,-5.31350540756609E-33,-0.674432891191581));
#21936=CARTESIAN_POINT('',(0.453126641287998,8.49470414473068E-34,-1.04559637023808));
#21937=CARTESIAN_POINT('Origin',(0.685838782044607,0.,-0.860014630714833));
#21938=CARTESIAN_POINT('Origin',(-0.244773027351946,0.,-1.07242070340001));
#21939=CARTESIAN_POINT('',(0.0454142657089739,-2.23201749654651E-33,-1.1386540593921));
#21940=CARTESIAN_POINT('',(-0.534960320412865,-2.23201749654651E-33,-1.00618734740791));
#21941=CARTESIAN_POINT('Origin',(-0.244773027351946,0.,-1.07242070340001));
#21942=CARTESIAN_POINT('Origin',(-0.991065754692661,0.,-0.477272113029314));
#21943=CARTESIAN_POINT('',(-0.86192025974432,8.49470414473067E-34,-0.745445496560469));
#21944=CARTESIAN_POINT('',(-1.120211249641,-5.31350540756609E-33,-0.209098729498159));
#21945=CARTESIAN_POINT('Origin',(-0.991065754692661,0.,-0.477272113029314));
#21946=CARTESIAN_POINT('Origin',(-0.991065754692661,0.,0.477272113029314));
#21947=CARTESIAN_POINT('',(-1.120211249641,-2.23201749654651E-33,0.209098729498159));
#21948=CARTESIAN_POINT('',(-0.86192025974432,-2.23201749654651E-33,0.745445496560469));
#21949=CARTESIAN_POINT('Origin',(-0.991065754692661,0.,0.477272113029314));
#21950=CARTESIAN_POINT('Origin',(-0.244773027351946,0.,1.07242070340001));
#21951=CARTESIAN_POINT('',(-0.534960320412866,-2.23201749654651E-33,1.00618734740791));
#21952=CARTESIAN_POINT('',(0.0454142657089737,-2.23201749654651E-33,1.1386540593921));
#21953=CARTESIAN_POINT('Origin',(-0.244773027351946,0.,1.07242070340001));
#21954=CARTESIAN_POINT('Origin',(0.685838782044607,0.,0.860014630714833));
#21955=CARTESIAN_POINT('',(0.453126641287998,-2.23201749654651E-33,1.04559637023808));
#21956=CARTESIAN_POINT('',(0.918550922801216,-2.23201749654651E-33,0.674432891191581));
#21957=CARTESIAN_POINT('Origin',(0.685838782044607,0.,0.860014630714833));
#21958=CARTESIAN_POINT('',(0.,0.,0.));
#21959=CARTESIAN_POINT('Origin',(0.685838782044607,0.,0.860014630714833));
#21960=CARTESIAN_POINT('',(0.413083465285518,-0.05953,0.993751811093549));
#21961=CARTESIAN_POINT('',(0.876916659919095,-0.05953,0.623857181492959));
#21962=CARTESIAN_POINT('Ctrl Pts',(0.413083465285518,-0.05953,0.993751811093549));
#21963=CARTESIAN_POINT('Ctrl Pts',(0.419070565453383,-0.0925528133349865,
0.991263089003441));
#21964=CARTESIAN_POINT('Ctrl Pts',(0.430199341854858,-0.124911173756694,
0.986608710139579));
#21965=CARTESIAN_POINT('Ctrl Pts',(0.457978755888596,-0.177924977804098,
0.973971221090534));
#21966=CARTESIAN_POINT('Ctrl Pts',(0.473077587363685,-0.199697230012983,
0.966820759530997));
#21967=CARTESIAN_POINT('Ctrl Pts',(0.507057380724533,-0.237895043532788,
0.949440676105255));
#21968=CARTESIAN_POINT('Ctrl Pts',(0.525933334162555,-0.254319232363049,
0.939198248544428));
#21969=CARTESIAN_POINT('Ctrl Pts',(0.564362943424238,-0.28018331644634,
0.916597376014514));
#21970=CARTESIAN_POINT('Ctrl Pts',(0.585840553788742,-0.29104845371857,
0.903141581680914));
#21971=CARTESIAN_POINT('Ctrl Pts',(0.629305439856167,-0.30527573347708,
0.873412008702649));
#21972=CARTESIAN_POINT('Ctrl Pts',(0.651278921914856,-0.308638795020976,
0.857118508332695));
#21973=CARTESIAN_POINT('Ctrl Pts',(0.690705563850638,-0.308638795020976,
0.825676810575914));
#21974=CARTESIAN_POINT('Ctrl Pts',(0.711480111898423,-0.30527573347708,
0.807879894508811));
#21975=CARTESIAN_POINT('Ctrl Pts',(0.750136149454208,-0.29104845371857,
0.772120216227122));
#21976=CARTESIAN_POINT('Ctrl Pts',(0.768033796848072,-0.28018331644634,
0.754175290318038));
#21977=CARTESIAN_POINT('Ctrl Pts',(0.798619410861634,-0.254319232363049,
0.721738358858166));
#21978=CARTESIAN_POINT('Ctrl Pts',(0.812805334167529,-0.237895043532788,
0.705614819529209));
#21979=CARTESIAN_POINT('Ctrl Pts',(0.837310877969633,-0.199697230012983,
0.676354402927683));
#21980=CARTESIAN_POINT('Ctrl Pts',(0.847641868610495,-0.177924977804098,
0.663225258065736));
#21981=CARTESIAN_POINT('Ctrl Pts',(0.866144010579847,-0.124911173756694,
0.638954437806245));
#21982=CARTESIAN_POINT('Ctrl Pts',(0.873158080166742,-0.0925528133349865,
0.62914037979579));
#21983=CARTESIAN_POINT('Ctrl Pts',(0.876916659919095,-0.05953,0.623857181492959));
#21984=CARTESIAN_POINT('',(0.437601487681057,-0.05953,1.03511272300331));
#21985=CARTESIAN_POINT('Origin',(0.685838782044607,-0.05953,0.860014630714833));
#21986=CARTESIAN_POINT('',(0.911784794170997,-0.05953,0.656964154625313));
#21987=CARTESIAN_POINT('Ctrl Pts',(0.911784794170998,-0.0595300000000001,
0.656964154625312));
#21988=CARTESIAN_POINT('Ctrl Pts',(0.909827729890942,-0.0762225747374255,
0.659680317203144));
#21989=CARTESIAN_POINT('Ctrl Pts',(0.907004864562642,-0.0928409665394228,
0.663576540841106));
#21990=CARTESIAN_POINT('Ctrl Pts',(0.895234408667242,-0.144299303100741,
0.679480524217551));
#21991=CARTESIAN_POINT('Ctrl Pts',(0.882797231409153,-0.177024326825049,
0.695831250979106));
#21992=CARTESIAN_POINT('Ctrl Pts',(0.854332839576145,-0.227269801620064,
0.73042219438957));
#21993=CARTESIAN_POINT('Ctrl Pts',(0.834863020612702,-0.251265615809407,
0.752807465209441));
#21994=CARTESIAN_POINT('Ctrl Pts',(0.800439809856111,-0.279889827963178,
0.789147407129766));
#21995=CARTESIAN_POINT('Ctrl Pts',(0.781998747691871,-0.290879136862659,
0.80756613568454));
#21996=CARTESIAN_POINT('Ctrl Pts',(0.742239891936898,-0.305251990234487,
0.844254137480382));
#21997=CARTESIAN_POINT('Ctrl Pts',(0.720906778729541,-0.308638795020976,
0.862505527716294));
#21998=CARTESIAN_POINT('Ctrl Pts',(0.680463863683392,-0.308638795020976,
0.894757676234429));
#21999=CARTESIAN_POINT('Ctrl Pts',(0.657923009631182,-0.305251990234488,
0.91149460735272));
#22000=CARTESIAN_POINT('Ctrl Pts',(0.613307674922609,-0.290879136862659,
0.942092777160053));
#22001=CARTESIAN_POINT('Ctrl Pts',(0.591247219971725,-0.279889827963178,
0.955972930713954));
#22002=CARTESIAN_POINT('Ctrl Pts',(0.548158511259202,-0.251265615809407,
0.981446681891443));
#22003=CARTESIAN_POINT('Ctrl Pts',(0.522002043615455,-0.227269801620063,
0.995447160474328));
#22004=CARTESIAN_POINT('Ctrl Pts',(0.481944444320713,-0.177024326825049,
1.01550068154148));
#22005=CARTESIAN_POINT('Ctrl Pts',(0.463236132117164,-0.14429930310074,
1.0239876538093));
#22006=CARTESIAN_POINT('Ctrl Pts',(0.445111721969657,-0.0928409665394226,
1.03192403056628));
#22007=CARTESIAN_POINT('Ctrl Pts',(0.440685038163619,-0.0762225747374254,
1.03380912944435));
#22008=CARTESIAN_POINT('Ctrl Pts',(0.437601487681056,-0.05953,1.03511272300331));
#22009=CARTESIAN_POINT('Origin',(0.685838782044607,-0.05953,0.860014630714833));
#22010=CARTESIAN_POINT('Origin',(0.,-0.208355,0.));
#22011=CARTESIAN_POINT('',(0.0548532617164168,-0.05953,1.12247250791415));
#22012=CARTESIAN_POINT('Origin',(0.,-0.05953,0.));
#22013=CARTESIAN_POINT('',(-0.536443649899848,-0.05953,0.987512846410683));
#22014=CARTESIAN_POINT('Ctrl Pts',(0.0548532617164173,-0.0595300000000001,
1.12247250791414));
#22015=CARTESIAN_POINT('Ctrl Pts',(0.05150947068137,-0.0762225747374254,
1.12263591311425));
#22016=CARTESIAN_POINT('Ctrl Pts',(0.0467032526342597,-0.0928409665394227,
1.12285816383385));
#22017=CARTESIAN_POINT('Ctrl Pts',(0.0269302585198975,-0.144299303100741,
1.12357162229597));
#22018=CARTESIAN_POINT('Ctrl Pts',(0.006392292392153,-0.177024326825049,
1.12404235695137));
#22019=CARTESIAN_POINT('Ctrl Pts',(-0.0383992541984087,-0.227269801620063,
1.12335509974011));
#22020=CARTESIAN_POINT('Ctrl Pts',(-0.0680399972366993,-0.251265615809407,
1.12208997038458));
#22021=CARTESIAN_POINT('Ctrl Pts',(-0.117914228755037,-0.279889827963178,
1.1178344036749));
#22022=CARTESIAN_POINT('Ctrl Pts',(-0.14381238480104,-0.290879136862659,
1.11490049012186));
#22023=CARTESIAN_POINT('Ctrl Pts',(-0.19728546073067,-0.305251990234488,
1.10669035995599));
#22024=CARTESIAN_POINT('Ctrl Pts',(-0.224855950742601,-0.308638795020976,
1.10139101611326));
#22025=CARTESIAN_POINT('Ctrl Pts',(-0.275287440920027,-0.308638795020976,
1.0898803575765));
#22026=CARTESIAN_POINT('Ctrl Pts',(-0.302426893214945,-0.305251990234488,
1.08269251410343));
#22027=CARTESIAN_POINT('Ctrl Pts',(-0.35416671187353,-0.290879136862659,
1.06688848765783));
#22028=CARTESIAN_POINT('Ctrl Pts',(-0.3787731215897,-0.279889827963178,
1.05829506364875));
#22029=CARTESIAN_POINT('Ctrl Pts',(-0.425554672694338,-0.251265615809407,
1.04048957871266));
#22030=CARTESIAN_POINT('Ctrl Pts',(-0.452808978448581,-0.227269801620063,
1.02876878445619));
#22031=CARTESIAN_POINT('Ctrl Pts',(-0.493462957200432,-0.177024326825049,
1.0099536580922));
#22032=CARTESIAN_POINT('Ctrl Pts',(-0.511762781179148,-0.14429930310074,
1.00061845128527));
#22033=CARTESIAN_POINT('Ctrl Pts',(-0.529268075276157,-0.0928409665394226,
0.991396466802468));
#22034=CARTESIAN_POINT('Ctrl Pts',(-0.533501897135713,-0.0762225747374254,
0.989110885965947));
#22035=CARTESIAN_POINT('Ctrl Pts',(-0.536443649899848,-0.0595300000000001,
0.987512846410683));
#22036=CARTESIAN_POINT('',(-0.843383895613249,-0.05953,0.742736168477219));
#22037=CARTESIAN_POINT('Origin',(0.,-0.05953,0.));
#22038=CARTESIAN_POINT('',(-1.10653577764992,-0.05953,0.196295654879792));
#22039=CARTESIAN_POINT('Ctrl Pts',(-0.843383895613249,-0.0595300000000001,
0.742736168477219));
#22040=CARTESIAN_POINT('Ctrl Pts',(-0.84559647055299,-0.0762225747374255,
0.740223768851062));
#22041=CARTESIAN_POINT('Ctrl Pts',(-0.848766861100456,-0.0928409665394227,
0.736604687327351));
#22042=CARTESIAN_POINT('Ctrl Pts',(-0.861652925570091,-0.144299303100741,
0.721590372101268));
#22043=CARTESIAN_POINT('Ctrl Pts',(-0.87482617317514,-0.177024326825049,
0.705826641853758));
#22044=CARTESIAN_POINT('Ctrl Pts',(-0.902215926359523,-0.227269801620063,
0.670378702718353));
#22045=CARTESIAN_POINT('Ctrl Pts',(-0.919707509403859,-0.251265615809407,
0.646415841396062));
#22046=CARTESIAN_POINT('Ctrl Pts',(-0.947476448101718,-0.279889827963178,
0.604769294586516));
#22047=CARTESIAN_POINT('Ctrl Pts',(-0.961329858300736,-0.290879136862659,
0.582692035672022));
#22048=CARTESIAN_POINT('Ctrl Pts',(-0.988250837578047,-0.305251990234488,
0.535766169015486));
#22049=CARTESIAN_POINT('Ctrl Pts',(-1.00129756308006,-0.308638795020976,
0.510906605094603));
#22050=CARTESIAN_POINT('Ctrl Pts',(-1.02374168767024,-0.308638795020976,
0.46430090015576));
#22051=CARTESIAN_POINT('Ctrl Pts',(-1.03504317708586,-0.305251990234488,
0.438600874831839));
#22052=CARTESIAN_POINT('Ctrl Pts',(-1.05494634094458,-0.290879136862659,
0.388295406390235));
#22053=CARTESIAN_POINT('Ctrl Pts',(-1.06356957703048,-0.279889827963178,
0.363699428370917));
#22054=CARTESIAN_POINT('Ctrl Pts',(-1.0788165083757,-0.251265615809407,
0.316022600643821));
#22055=CARTESIAN_POINT('Ctrl Pts',(-1.08664560412098,-0.227269801620063,
0.287406530683752));
#22056=CARTESIAN_POINT('Ctrl Pts',(-1.09728268713976,-0.177024326825049,
0.243890930799337));
#22057=CARTESIAN_POINT('Ctrl Pts',(-1.10139388218929,-0.144299303100741,
0.22376314604679));
#22058=CARTESIAN_POINT('Ctrl Pts',(-1.10509821673782,-0.0928409665394227,
0.204327142733961));
#22059=CARTESIAN_POINT('Ctrl Pts',(-1.10595102243643,-0.0762225747374254,
0.199591971170104));
#22060=CARTESIAN_POINT('Ctrl Pts',(-1.10653577764992,-0.0595300000000001,
0.196295654879792));
#22061=CARTESIAN_POINT('',(-1.123812,-0.05953,1.37627276864339E-16));
#22062=CARTESIAN_POINT('Origin',(0.,-0.05953,0.));
#22063=CARTESIAN_POINT('',(-1.123812,-0.35718,1.37627276864339E-16));
#22064=CARTESIAN_POINT('',(-1.123812,-0.208355,1.37627276864339E-16));
#22065=CARTESIAN_POINT('Origin',(0.,-0.35718,0.));
#22066=CARTESIAN_POINT('',(-1.10653577764992,-0.05953,-0.196295654879793));
#22067=CARTESIAN_POINT('Origin',(0.,-0.05953,0.));
#22068=CARTESIAN_POINT('',(-0.843383895613249,-0.05953,-0.742736168477219));
#22069=CARTESIAN_POINT('Ctrl Pts',(-1.10653577764992,-0.0595300000000001,
-0.196295654879792));
#22070=CARTESIAN_POINT('Ctrl Pts',(-1.10595102243643,-0.0762225747374255,
-0.199591971170104));
#22071=CARTESIAN_POINT('Ctrl Pts',(-1.10509821673782,-0.0928409665394228,
-0.204327142733962));
#22072=CARTESIAN_POINT('Ctrl Pts',(-1.10139388218929,-0.144299303100741,
-0.22376314604679));
#22073=CARTESIAN_POINT('Ctrl Pts',(-1.09728268713976,-0.177024326825049,
-0.243890930799338));
#22074=CARTESIAN_POINT('Ctrl Pts',(-1.08664560412098,-0.227269801620063,
-0.287406530683753));
#22075=CARTESIAN_POINT('Ctrl Pts',(-1.0788165083757,-0.251265615809407,
-0.316022600643821));
#22076=CARTESIAN_POINT('Ctrl Pts',(-1.06356957703048,-0.279889827963178,
-0.363699428370918));
#22077=CARTESIAN_POINT('Ctrl Pts',(-1.05494634094458,-0.290879136862659,
-0.388295406390235));
#22078=CARTESIAN_POINT('Ctrl Pts',(-1.03504317708586,-0.305251990234488,
-0.438600874831839));
#22079=CARTESIAN_POINT('Ctrl Pts',(-1.02374168767024,-0.308638795020976,
-0.46430090015576));
#22080=CARTESIAN_POINT('Ctrl Pts',(-1.00129756308006,-0.308638795020976,
-0.510906605094603));
#22081=CARTESIAN_POINT('Ctrl Pts',(-0.988250837578047,-0.305251990234488,
-0.535766169015486));
#22082=CARTESIAN_POINT('Ctrl Pts',(-0.961329858300736,-0.290879136862659,
-0.582692035672022));
#22083=CARTESIAN_POINT('Ctrl Pts',(-0.947476448101718,-0.279889827963178,
-0.604769294586516));
#22084=CARTESIAN_POINT('Ctrl Pts',(-0.919707509403859,-0.251265615809407,
-0.646415841396062));
#22085=CARTESIAN_POINT('Ctrl Pts',(-0.902215926359523,-0.227269801620064,
-0.670378702718353));
#22086=CARTESIAN_POINT('Ctrl Pts',(-0.87482617317514,-0.177024326825049,
-0.705826641853758));
#22087=CARTESIAN_POINT('Ctrl Pts',(-0.861652925570091,-0.144299303100741,
-0.721590372101268));
#22088=CARTESIAN_POINT('Ctrl Pts',(-0.848766861100456,-0.0928409665394229,
-0.736604687327351));
#22089=CARTESIAN_POINT('Ctrl Pts',(-0.84559647055299,-0.0762225747374255,
-0.740223768851063));
#22090=CARTESIAN_POINT('Ctrl Pts',(-0.843383895613249,-0.0595300000000001,
-0.742736168477219));
#22091=CARTESIAN_POINT('',(-0.536443649899847,-0.05953,-0.987512846410683));
#22092=CARTESIAN_POINT('Origin',(0.,-0.05953,0.));
#22093=CARTESIAN_POINT('',(0.0548532617164172,-0.05953,-1.12247250791415));
#22094=CARTESIAN_POINT('Ctrl Pts',(-0.536443649899848,-0.0595300000000001,
-0.987512846410683));
#22095=CARTESIAN_POINT('Ctrl Pts',(-0.533501897135712,-0.0762225747374254,
-0.989110885965947));
#22096=CARTESIAN_POINT('Ctrl Pts',(-0.529268075276156,-0.0928409665394227,
-0.991396466802469));
#22097=CARTESIAN_POINT('Ctrl Pts',(-0.511762781179147,-0.144299303100741,
-1.00061845128527));
#22098=CARTESIAN_POINT('Ctrl Pts',(-0.493462957200432,-0.177024326825049,
-1.0099536580922));
#22099=CARTESIAN_POINT('Ctrl Pts',(-0.45280897844858,-0.227269801620063,
-1.02876878445619));
#22100=CARTESIAN_POINT('Ctrl Pts',(-0.425554672694337,-0.251265615809407,
-1.04048957871266));
#22101=CARTESIAN_POINT('Ctrl Pts',(-0.3787731215897,-0.279889827963178,
-1.05829506364875));
#22102=CARTESIAN_POINT('Ctrl Pts',(-0.354166711873529,-0.290879136862659,
-1.06688848765783));
#22103=CARTESIAN_POINT('Ctrl Pts',(-0.302426893214944,-0.305251990234488,
-1.08269251410343));
#22104=CARTESIAN_POINT('Ctrl Pts',(-0.275287440920027,-0.308638795020976,
-1.0898803575765));
#22105=CARTESIAN_POINT('Ctrl Pts',(-0.224855950742601,-0.308638795020976,
-1.10139101611326));
#22106=CARTESIAN_POINT('Ctrl Pts',(-0.19728546073067,-0.305251990234488,
-1.10669035995599));
#22107=CARTESIAN_POINT('Ctrl Pts',(-0.143812384801039,-0.290879136862659,
-1.11490049012186));
#22108=CARTESIAN_POINT('Ctrl Pts',(-0.117914228755037,-0.279889827963178,
-1.1178344036749));
#22109=CARTESIAN_POINT('Ctrl Pts',(-0.0680399972366989,-0.251265615809407,
-1.12208997038458));
#22110=CARTESIAN_POINT('Ctrl Pts',(-0.0383992541984084,-0.227269801620063,
-1.12335509974011));
#22111=CARTESIAN_POINT('Ctrl Pts',(0.00639229239215326,-0.177024326825049,
-1.12404235695137));
#22112=CARTESIAN_POINT('Ctrl Pts',(0.0269302585198977,-0.144299303100741,
-1.12357162229597));
#22113=CARTESIAN_POINT('Ctrl Pts',(0.04670325263426,-0.0928409665394228,
-1.12285816383385));
#22114=CARTESIAN_POINT('Ctrl Pts',(0.0515094706813703,-0.0762225747374255,
-1.12263591311425));
#22115=CARTESIAN_POINT('Ctrl Pts',(0.0548532617164176,-0.0595300000000001,
-1.12247250791414));
#22116=CARTESIAN_POINT('',(0.437601487681057,-0.05953,-1.03511272300331));
#22117=CARTESIAN_POINT('Origin',(0.,-0.05953,0.));
#22118=CARTESIAN_POINT('',(0.911784794170997,-0.05953,-0.656964154625313));
#22119=CARTESIAN_POINT('Ctrl Pts',(0.437601487681056,-0.0595300000000001,
-1.03511272300331));
#22120=CARTESIAN_POINT('Ctrl Pts',(0.440685038163619,-0.0762225747374255,
-1.03380912944435));
#22121=CARTESIAN_POINT('Ctrl Pts',(0.445111721969657,-0.0928409665394228,
-1.03192403056628));
#22122=CARTESIAN_POINT('Ctrl Pts',(0.463236132117164,-0.144299303100741,
-1.0239876538093));
#22123=CARTESIAN_POINT('Ctrl Pts',(0.481944444320713,-0.177024326825049,
-1.01550068154148));
#22124=CARTESIAN_POINT('Ctrl Pts',(0.522002043615455,-0.227269801620064,
-0.995447160474328));
#22125=CARTESIAN_POINT('Ctrl Pts',(0.548158511259203,-0.251265615809407,
-0.981446681891443));
#22126=CARTESIAN_POINT('Ctrl Pts',(0.591247219971725,-0.279889827963178,
-0.955972930713954));
#22127=CARTESIAN_POINT('Ctrl Pts',(0.613307674922609,-0.290879136862659,
-0.942092777160053));
#22128=CARTESIAN_POINT('Ctrl Pts',(0.657923009631182,-0.305251990234487,
-0.91149460735272));
#22129=CARTESIAN_POINT('Ctrl Pts',(0.680463863683393,-0.308638795020976,
-0.894757676234429));
#22130=CARTESIAN_POINT('Ctrl Pts',(0.720906778729542,-0.308638795020976,
-0.862505527716294));
#22131=CARTESIAN_POINT('Ctrl Pts',(0.742239891936899,-0.305251990234488,
-0.844254137480381));
#22132=CARTESIAN_POINT('Ctrl Pts',(0.781998747691872,-0.290879136862659,
-0.80756613568454));
#22133=CARTESIAN_POINT('Ctrl Pts',(0.800439809856112,-0.279889827963178,
-0.789147407129765));
#22134=CARTESIAN_POINT('Ctrl Pts',(0.834863020612702,-0.251265615809407,
-0.752807465209441));
#22135=CARTESIAN_POINT('Ctrl Pts',(0.854332839576145,-0.227269801620064,
-0.73042219438957));
#22136=CARTESIAN_POINT('Ctrl Pts',(0.882797231409153,-0.177024326825049,
-0.695831250979106));
#22137=CARTESIAN_POINT('Ctrl Pts',(0.895234408667242,-0.144299303100741,
-0.679480524217551));
#22138=CARTESIAN_POINT('Ctrl Pts',(0.907004864562642,-0.0928409665394228,
-0.663576540841106));
#22139=CARTESIAN_POINT('Ctrl Pts',(0.909827729890942,-0.0762225747374256,
-0.659680317203144));
#22140=CARTESIAN_POINT('Ctrl Pts',(0.911784794170998,-0.0595300000000001,
-0.656964154625312));
#22141=CARTESIAN_POINT('',(1.08212377959455,-0.05953,-0.303251606722892));
#22142=CARTESIAN_POINT('Origin',(0.,-0.05953,0.));
#22143=CARTESIAN_POINT('',(1.08212377959455,-0.05953,0.303251606722892));
#22144=CARTESIAN_POINT('Ctrl Pts',(1.08212377959455,-0.0595300000000001,
-0.303251606722892));
#22145=CARTESIAN_POINT('Ctrl Pts',(1.0830271513892,-0.0762225747374255,
-0.300028012588062));
#22146=CARTESIAN_POINT('Ctrl Pts',(1.08431331394788,-0.0928409665394228,
-0.2953917518996));
#22147=CARTESIAN_POINT('Ctrl Pts',(1.08940878963422,-0.144299303100741,
-0.276273267473431));
#22148=CARTESIAN_POINT('Ctrl Pts',(1.09443784939331,-0.177024326825049,
-0.256354979351213));
#22149=CARTESIAN_POINT('Ctrl Pts',(1.10373487993589,-0.227269801620064,
-0.212533521233765));
#22150=CARTESIAN_POINT('Ctrl Pts',(1.10909715583869,-0.251265615809407,
-0.183354415742157));
#22151=CARTESIAN_POINT('Ctrl Pts',(1.1160463456491,-0.279889827963178,-0.133783682657561));
#22152=CARTESIAN_POINT('Ctrl Pts',(1.11894887330541,-0.290879136862659,
-0.107881990270302));
#22153=CARTESIAN_POINT('Ctrl Pts',(1.12284346704144,-0.305251990234488,
-0.0539226701638766));
#22154=CARTESIAN_POINT('Ctrl Pts',(1.123812,-0.308638795020976,-0.025864214957475));
#22155=CARTESIAN_POINT('Ctrl Pts',(1.123812,-0.308638795020976,0.025864214957475));
#22156=CARTESIAN_POINT('Ctrl Pts',(1.12284346704144,-0.305251990234488,
0.0539226701638766));
#22157=CARTESIAN_POINT('Ctrl Pts',(1.11894887330541,-0.290879136862659,
0.107881990270302));
#22158=CARTESIAN_POINT('Ctrl Pts',(1.1160463456491,-0.279889827963178,0.133783682657561));
#22159=CARTESIAN_POINT('Ctrl Pts',(1.10909715583869,-0.251265615809407,
0.183354415742157));
#22160=CARTESIAN_POINT('Ctrl Pts',(1.10373487993589,-0.227269801620064,
0.212533521233765));
#22161=CARTESIAN_POINT('Ctrl Pts',(1.09443784939331,-0.177024326825049,
0.256354979351213));
#22162=CARTESIAN_POINT('Ctrl Pts',(1.08940878963422,-0.144299303100741,
0.276273267473431));
#22163=CARTESIAN_POINT('Ctrl Pts',(1.08431331394788,-0.0928409665394228,
0.2953917518996));
#22164=CARTESIAN_POINT('Ctrl Pts',(1.0830271513892,-0.0762225747374255,
0.300028012588062));
#22165=CARTESIAN_POINT('Ctrl Pts',(1.08212377959455,-0.0595300000000001,
0.303251606722892));
#22166=CARTESIAN_POINT('Origin',(0.,-0.05953,0.));
#22167=CARTESIAN_POINT('Origin',(0.,-0.05953,0.));
#22168=CARTESIAN_POINT('',(0.0589974094846122,-0.05953,1.07456964270265));
#22169=CARTESIAN_POINT('Origin',(0.,-0.05953,0.));
#22170=CARTESIAN_POINT('Origin',(-0.244773027351946,-0.05953,1.07242070340001));
#22171=CARTESIAN_POINT('Origin',(-0.244773027351946,0.,1.07242070340001));
#22172=CARTESIAN_POINT('',(-0.519393123750572,-0.05953,0.942555777842682));
#22173=CARTESIAN_POINT('Ctrl Pts',(-0.519393123750572,-0.05953,0.942555777842682));
#22174=CARTESIAN_POINT('Ctrl Pts',(-0.513714466572041,-0.0925528133349865,
0.945684988399766));
#22175=CARTESIAN_POINT('Ctrl Pts',(-0.503136848051455,-0.124911173756694,
0.951483858396181));
#22176=CARTESIAN_POINT('Ctrl Pts',(-0.47593627990192,-0.177924977804098,
0.965323333309091));
#22177=CARTESIAN_POINT('Ctrl Pts',(-0.460931856495794,-0.199697230012983,
0.972669835243841));
#22178=CARTESIAN_POINT('Ctrl Pts',(-0.426157505475872,-0.237895043532788,
0.988400002689705));
#22179=CARTESIAN_POINT('Ctrl Pts',(-0.406380688682952,-0.254319232363049,
0.996771768218699));
#22180=CARTESIAN_POINT('Ctrl Pts',(-0.364750145543744,-0.28018331644634,
1.01272583306292));
#22181=CARTESIAN_POINT('Ctrl Pts',(-0.340838910881557,-0.29104845371857,
1.02112815447116));
#22182=CARTESIAN_POINT('Ctrl Pts',(-0.290495481564827,-0.30527573347708,
1.036574285215));
#22183=CARTESIAN_POINT('Ctrl Pts',(-0.264056468041074,-0.308638795020976,
1.04359501395068));
#22184=CARTESIAN_POINT('Ctrl Pts',(-0.214892249704082,-0.308638795020976,
1.05481642595959));
#22185=CARTESIAN_POINT('Ctrl Pts',(-0.188025341585962,-0.30527573347708,
1.05996242598502));
#22186=CARTESIAN_POINT('Ctrl Pts',(-0.135965654106109,-0.29104845371857,
1.06788913840721));
#22187=CARTESIAN_POINT('Ctrl Pts',(-0.110776745452494,-0.28018331644634,
1.07069360430242));
#22188=CARTESIAN_POINT('Ctrl Pts',(-0.0663467128214646,-0.254319232363049,
1.07438230428002));
#22189=CARTESIAN_POINT('Ctrl Pts',(-0.0448960436540983,-0.237895043532788,
1.07542044338697));
#22190=CARTESIAN_POINT('Ctrl Pts',(-0.00674037211528124,-0.199697230012983,
1.07633607767727));
#22191=CARTESIAN_POINT('Ctrl Pts',(0.00996567398334777,-0.177924977804098,
1.07622728347683));
#22192=CARTESIAN_POINT('Ctrl Pts',(0.0404772621979741,-0.124911173756694,
1.07556023164702));
#22193=CARTESIAN_POINT('Ctrl Pts',(0.0525234025782719,-0.0925528133349865,
1.07492508698591));
#22194=CARTESIAN_POINT('Ctrl Pts',(0.0589974094846124,-0.05953,1.07456964270265));
#22195=CARTESIAN_POINT('Origin',(-0.244773027351946,-0.05953,1.07242070340001));
#22196=CARTESIAN_POINT('Origin',(0.,-0.05953,0.));
#22197=CARTESIAN_POINT('',(-0.803348093619616,-0.05953,0.716109245731214));
#22198=CARTESIAN_POINT('Origin',(0.,-0.05953,0.));
#22199=CARTESIAN_POINT('Origin',(-0.991065754692661,-0.05953,0.477272113029314));
#22200=CARTESIAN_POINT('Origin',(-0.991065754692661,0.,0.477272113029314));
#22201=CARTESIAN_POINT('',(-1.06075609691358,-0.05953,0.181596019242328));
#22202=CARTESIAN_POINT('Ctrl Pts',(-1.06075609691358,-0.05953,0.181596019242328));
#22203=CARTESIAN_POINT('Ctrl Pts',(-1.05966202740332,-0.0925528133349865,
0.187986803072856));
#22204=CARTESIAN_POINT('Ctrl Pts',(-1.05760072925372,-0.124911173756694,
0.199872254546857));
#22205=CARTESIAN_POINT('Ctrl Pts',(-1.05146158959546,-0.177924977804098,
0.22976728653846));
#22206=CARTESIAN_POINT('Ctrl Pts',(-1.04785021111757,-0.199697230012983,
0.246078686169301));
#22207=CARTESIAN_POINT('Ctrl Pts',(-1.03846709802406,-0.237895043532788,
0.283073967563097));
#22208=CARTESIAN_POINT('Ctrl Pts',(-1.03268176429485,-0.254319232363049,
0.303755815985685));
#22209=CARTESIAN_POINT('Ctrl Pts',(-1.01919893537026,-0.28018331644634,
0.346251081972725));
#22210=CARTESIAN_POINT('Ctrl Pts',(-1.01085972381132,-0.29104845371857,
0.370184399726282));
#22211=CARTESIAN_POINT('Ctrl Pts',(-0.99154738033959,-0.30527573347708,
0.419174982698463));
#22212=CARTESIAN_POINT('Ctrl Pts',(-0.980551951791748,-0.308638795020976,
0.444223188605045));
#22213=CARTESIAN_POINT('Ctrl Pts',(-0.958671816228589,-0.308638795020976,
0.489657758261848));
#22214=CARTESIAN_POINT('Ctrl Pts',(-0.945943877838127,-0.30527573347708,
0.51387163140139));
#22215=CARTESIAN_POINT('Ctrl Pts',(-0.91968254693063,-0.29104845371857,
0.559515758398093));
#22216=CARTESIAN_POINT('Ctrl Pts',(-0.906170138993533,-0.28018331644634,
0.580957796077825));
#22217=CARTESIAN_POINT('Ctrl Pts',(-0.8813524085237,-0.254319232363049,
0.617994461173994));
#22218=CARTESIAN_POINT('Ctrl Pts',(-0.868789784891799,-0.237895043532788,
0.635412538795143));
#22219=CARTESIAN_POINT('Ctrl Pts',(-0.845715984518854,-0.199697230012983,
0.66581473268113));
#22220=CARTESIAN_POINT('Ctrl Pts',(-0.835214876415962,-0.177924977804098,
0.678808213394124));
#22221=CARTESIAN_POINT('Ctrl Pts',(-0.815669690204649,-0.124911173756694,
0.702247233627224));
#22222=CARTESIAN_POINT('Ctrl Pts',(-0.807662468433796,-0.0925528133349865,
0.711269279199861));
#22223=CARTESIAN_POINT('Ctrl Pts',(-0.803348093619616,-0.05953,0.716109245731214));
#22224=CARTESIAN_POINT('Origin',(-0.991065754692661,-0.05953,0.477272113029314));
#22225=CARTESIAN_POINT('Origin',(0.,-0.05953,0.));
#22226=CARTESIAN_POINT('',(-1.076188,-0.05953,1.31795018948079E-16));
#22227=CARTESIAN_POINT('Origin',(0.,-0.05953,0.));
#22228=CARTESIAN_POINT('',(-1.06075609691358,-0.05953,-0.181596019242328));
#22229=CARTESIAN_POINT('Origin',(0.,-0.05953,0.));
#22230=CARTESIAN_POINT('Origin',(-0.991065754692661,-0.05953,-0.477272113029314));
#22231=CARTESIAN_POINT('Origin',(-0.991065754692661,0.,-0.477272113029314));
#22232=CARTESIAN_POINT('',(-0.803348093619616,-0.05953,-0.716109245731215));
#22233=CARTESIAN_POINT('Ctrl Pts',(-0.803348093619616,-0.05953,-0.716109245731215));
#22234=CARTESIAN_POINT('Ctrl Pts',(-0.807662468433795,-0.0925528133349865,
-0.711269279199862));
#22235=CARTESIAN_POINT('Ctrl Pts',(-0.815669690204649,-0.124911173756694,
-0.702247233627224));
#22236=CARTESIAN_POINT('Ctrl Pts',(-0.835214876415962,-0.177924977804098,
-0.678808213394124));
#22237=CARTESIAN_POINT('Ctrl Pts',(-0.845715984518854,-0.199697230012983,
-0.66581473268113));
#22238=CARTESIAN_POINT('Ctrl Pts',(-0.868789784891799,-0.237895043532788,
-0.635412538795143));
#22239=CARTESIAN_POINT('Ctrl Pts',(-0.8813524085237,-0.254319232363049,
-0.617994461173994));
#22240=CARTESIAN_POINT('Ctrl Pts',(-0.906170138993533,-0.28018331644634,
-0.580957796077826));
#22241=CARTESIAN_POINT('Ctrl Pts',(-0.91968254693063,-0.29104845371857,
-0.559515758398093));
#22242=CARTESIAN_POINT('Ctrl Pts',(-0.945943877838127,-0.30527573347708,
-0.51387163140139));
#22243=CARTESIAN_POINT('Ctrl Pts',(-0.958671816228589,-0.308638795020976,
-0.489657758261848));
#22244=CARTESIAN_POINT('Ctrl Pts',(-0.980551951791748,-0.308638795020976,
-0.444223188605045));
#22245=CARTESIAN_POINT('Ctrl Pts',(-0.99154738033959,-0.30527573347708,
-0.419174982698463));
#22246=CARTESIAN_POINT('Ctrl Pts',(-1.01085972381132,-0.29104845371857,
-0.370184399726282));
#22247=CARTESIAN_POINT('Ctrl Pts',(-1.01919893537026,-0.28018331644634,
-0.346251081972725));
#22248=CARTESIAN_POINT('Ctrl Pts',(-1.03268176429485,-0.254319232363049,
-0.303755815985685));
#22249=CARTESIAN_POINT('Ctrl Pts',(-1.03846709802406,-0.237895043532788,
-0.283073967563097));
#22250=CARTESIAN_POINT('Ctrl Pts',(-1.04785021111757,-0.199697230012983,
-0.246078686169302));
#22251=CARTESIAN_POINT('Ctrl Pts',(-1.05146158959546,-0.177924977804098,
-0.229767286538461));
#22252=CARTESIAN_POINT('Ctrl Pts',(-1.05760072925372,-0.124911173756694,
-0.199872254546858));
#22253=CARTESIAN_POINT('Ctrl Pts',(-1.05966202740332,-0.0925528133349864,
-0.187986803072857));
#22254=CARTESIAN_POINT('Ctrl Pts',(-1.06075609691358,-0.05953,-0.181596019242328));
#22255=CARTESIAN_POINT('Origin',(-0.991065754692661,-0.05953,-0.477272113029314));
#22256=CARTESIAN_POINT('Origin',(0.,-0.05953,0.));
#22257=CARTESIAN_POINT('',(-0.519393123750572,-0.05953,-0.942555777842682));
#22258=CARTESIAN_POINT('Origin',(0.,-0.05953,0.));
#22259=CARTESIAN_POINT('Origin',(-0.244773027351946,-0.05953,-1.07242070340001));
#22260=CARTESIAN_POINT('Origin',(-0.244773027351946,0.,-1.07242070340001));
#22261=CARTESIAN_POINT('',(0.0589974094846125,-0.05953,-1.07456964270265));
#22262=CARTESIAN_POINT('Ctrl Pts',(0.0589974094846127,-0.05953,-1.07456964270265));
#22263=CARTESIAN_POINT('Ctrl Pts',(0.0525234025782722,-0.0925528133349865,
-1.07492508698591));
#22264=CARTESIAN_POINT('Ctrl Pts',(0.0404772621979744,-0.124911173756694,
-1.07556023164702));
#22265=CARTESIAN_POINT('Ctrl Pts',(0.0099656739833481,-0.177924977804098,
-1.07622728347683));
#22266=CARTESIAN_POINT('Ctrl Pts',(-0.00674037211528096,-0.199697230012983,
-1.07633607767727));
#22267=CARTESIAN_POINT('Ctrl Pts',(-0.044896043654098,-0.237895043532788,
-1.07542044338697));
#22268=CARTESIAN_POINT('Ctrl Pts',(-0.0663467128214644,-0.254319232363049,
-1.07438230428002));
#22269=CARTESIAN_POINT('Ctrl Pts',(-0.110776745452493,-0.28018331644634,
-1.07069360430242));
#22270=CARTESIAN_POINT('Ctrl Pts',(-0.135965654106109,-0.29104845371857,
-1.06788913840721));
#22271=CARTESIAN_POINT('Ctrl Pts',(-0.188025341585962,-0.30527573347708,
-1.05996242598502));
#22272=CARTESIAN_POINT('Ctrl Pts',(-0.214892249704082,-0.308638795020976,
-1.05481642595959));
#22273=CARTESIAN_POINT('Ctrl Pts',(-0.264056468041074,-0.308638795020976,
-1.04359501395068));
#22274=CARTESIAN_POINT('Ctrl Pts',(-0.290495481564827,-0.30527573347708,
-1.036574285215));
#22275=CARTESIAN_POINT('Ctrl Pts',(-0.340838910881557,-0.291048453718569,
-1.02112815447116));
#22276=CARTESIAN_POINT('Ctrl Pts',(-0.364750145543744,-0.28018331644634,
-1.01272583306292));
#22277=CARTESIAN_POINT('Ctrl Pts',(-0.406380688682952,-0.254319232363049,
-0.996771768218699));
#22278=CARTESIAN_POINT('Ctrl Pts',(-0.426157505475872,-0.237895043532788,
-0.988400002689705));
#22279=CARTESIAN_POINT('Ctrl Pts',(-0.460931856495794,-0.199697230012983,
-0.972669835243841));
#22280=CARTESIAN_POINT('Ctrl Pts',(-0.475936279901919,-0.177924977804098,
-0.965323333309091));
#22281=CARTESIAN_POINT('Ctrl Pts',(-0.503136848051454,-0.124911173756694,
-0.951483858396181));
#22282=CARTESIAN_POINT('Ctrl Pts',(-0.513714466572041,-0.0925528133349865,
-0.945684988399766));
#22283=CARTESIAN_POINT('Ctrl Pts',(-0.519393123750572,-0.05953,-0.942555777842682));
#22284=CARTESIAN_POINT('Origin',(-0.244773027351946,-0.05953,-1.07242070340001));
#22285=CARTESIAN_POINT('Origin',(0.,-0.05953,0.));
#22286=CARTESIAN_POINT('',(0.413083465285518,-0.05953,-0.993751811093549));
#22287=CARTESIAN_POINT('Origin',(0.,-0.05953,0.));
#22288=CARTESIAN_POINT('Origin',(0.685838782044607,-0.05953,-0.860014630714833));
#22289=CARTESIAN_POINT('Origin',(0.685838782044607,0.,-0.860014630714833));
#22290=CARTESIAN_POINT('',(0.876916659919095,-0.05953,-0.623857181492959));
#22291=CARTESIAN_POINT('Ctrl Pts',(0.876916659919095,-0.05953,-0.623857181492958));
#22292=CARTESIAN_POINT('Ctrl Pts',(0.873158080166742,-0.0925528133349865,
-0.62914037979579));
#22293=CARTESIAN_POINT('Ctrl Pts',(0.866144010579847,-0.124911173756694,
-0.638954437806245));
#22294=CARTESIAN_POINT('Ctrl Pts',(0.847641868610495,-0.177924977804098,
-0.663225258065736));
#22295=CARTESIAN_POINT('Ctrl Pts',(0.837310877969633,-0.199697230012983,
-0.676354402927683));
#22296=CARTESIAN_POINT('Ctrl Pts',(0.81280533416753,-0.237895043532788,
-0.705614819529209));
#22297=CARTESIAN_POINT('Ctrl Pts',(0.798619410861634,-0.254319232363049,
-0.721738358858166));
#22298=CARTESIAN_POINT('Ctrl Pts',(0.768033796848072,-0.28018331644634,
-0.754175290318038));
#22299=CARTESIAN_POINT('Ctrl Pts',(0.750136149454208,-0.29104845371857,
-0.772120216227122));
#22300=CARTESIAN_POINT('Ctrl Pts',(0.711480111898423,-0.30527573347708,
-0.807879894508811));
#22301=CARTESIAN_POINT('Ctrl Pts',(0.690705563850638,-0.308638795020976,
-0.825676810575913));
#22302=CARTESIAN_POINT('Ctrl Pts',(0.651278921914856,-0.308638795020976,
-0.857118508332695));
#22303=CARTESIAN_POINT('Ctrl Pts',(0.629305439856167,-0.30527573347708,
-0.873412008702649));
#22304=CARTESIAN_POINT('Ctrl Pts',(0.585840553788742,-0.29104845371857,
-0.903141581680914));
#22305=CARTESIAN_POINT('Ctrl Pts',(0.564362943424239,-0.28018331644634,
-0.916597376014514));
#22306=CARTESIAN_POINT('Ctrl Pts',(0.525933334162556,-0.254319232363049,
-0.939198248544427));
#22307=CARTESIAN_POINT('Ctrl Pts',(0.507057380724533,-0.237895043532788,
-0.949440676105255));
#22308=CARTESIAN_POINT('Ctrl Pts',(0.473077587363686,-0.199697230012983,
-0.966820759530997));
#22309=CARTESIAN_POINT('Ctrl Pts',(0.457978755888596,-0.177924977804098,
-0.973971221090534));
#22310=CARTESIAN_POINT('Ctrl Pts',(0.430199341854858,-0.124911173756694,
-0.986608710139579));
#22311=CARTESIAN_POINT('Ctrl Pts',(0.419070565453384,-0.0925528133349865,
-0.991263089003441));
#22312=CARTESIAN_POINT('Ctrl Pts',(0.413083465285518,-0.05953,-0.993751811093549));
#22313=CARTESIAN_POINT('Origin',(0.685838782044607,-0.05953,-0.860014630714833));
#22314=CARTESIAN_POINT('Origin',(0.,-0.208355,0.));
#22315=CARTESIAN_POINT('',(-1.076188,-0.35718,1.31795018948079E-16));
#22316=CARTESIAN_POINT('Origin',(0.,-0.35718,0.));
#22317=CARTESIAN_POINT('',(-1.076188,-0.208355,1.31795018948079E-16));
#22318=CARTESIAN_POINT('',(1.03449977959455,-0.05953,0.296632461748266));
#22319=CARTESIAN_POINT('Origin',(0.,-0.05953,0.));
#22320=CARTESIAN_POINT('',(1.03449977959455,-0.05953,-0.296632461748266));
#22321=CARTESIAN_POINT('Ctrl Pts',(1.03449977959455,-0.05953,0.296632461748267));
#22322=CARTESIAN_POINT('Ctrl Pts',(1.03628691421076,-0.0925528133349865,
0.290399865505497));
#22323=CARTESIAN_POINT('Ctrl Pts',(1.03958665287714,-0.124911173756694,
0.278797079997872));
#22324=CARTESIAN_POINT('Ctrl Pts',(1.0470264474309,-0.177924977804098,0.249198913998601));
#22325=CARTESIAN_POINT('Ctrl Pts',(1.05084995891418,-0.199697230012983,
0.232935932341942));
#22326=CARTESIAN_POINT('Ctrl Pts',(1.05844771715377,-0.237895043532788,
0.195533155353269));
#22327=CARTESIAN_POINT('Ctrl Pts',(1.06220882929878,-0.254319232363049,
0.17438929156337));
#22328=CARTESIAN_POINT('Ctrl Pts',(1.06849922508772,-0.28018331644634,0.130252399648131));
#22329=CARTESIAN_POINT('Ctrl Pts',(1.07137013248666,-0.29104845371857,0.105070977154072));
#22330=CARTESIAN_POINT('Ctrl Pts',(1.07522652957392,-0.30527573347708,0.0525526752791107));
#22331=CARTESIAN_POINT('Ctrl Pts',(1.076188,-0.308638795020976,0.025214283908933));
#22332=CARTESIAN_POINT('Ctrl Pts',(1.076188,-0.308638795020976,-0.025214283908933));
#22333=CARTESIAN_POINT('Ctrl Pts',(1.07522652957392,-0.30527573347708,-0.0525526752791107));
#22334=CARTESIAN_POINT('Ctrl Pts',(1.07137013248666,-0.29104845371857,-0.105070977154072));
#22335=CARTESIAN_POINT('Ctrl Pts',(1.06849922508772,-0.28018331644634,-0.130252399648131));
#22336=CARTESIAN_POINT('Ctrl Pts',(1.06220882929878,-0.254319232363049,
-0.17438929156337));
#22337=CARTESIAN_POINT('Ctrl Pts',(1.05844771715377,-0.237895043532788,
-0.195533155353269));
#22338=CARTESIAN_POINT('Ctrl Pts',(1.05084995891418,-0.199697230012983,
-0.232935932341942));
#22339=CARTESIAN_POINT('Ctrl Pts',(1.0470264474309,-0.177924977804098,-0.249198913998601));
#22340=CARTESIAN_POINT('Ctrl Pts',(1.03958665287714,-0.124911173756694,
-0.278797079997872));
#22341=CARTESIAN_POINT('Ctrl Pts',(1.03628691421076,-0.0925528133349865,
-0.290399865505497));
#22342=CARTESIAN_POINT('Ctrl Pts',(1.03449977959455,-0.05953,-0.296632461748267));
#22343=CARTESIAN_POINT('Origin',(0.,-0.05953,0.));
#22344=CARTESIAN_POINT('Origin',(0.,-0.05953,0.));
#22345=CARTESIAN_POINT('Origin',(1.1,-0.05953,0.));
#22346=CARTESIAN_POINT('Origin',(1.1,0.,0.));
#22347=CARTESIAN_POINT('Origin',(1.1,-0.05953,0.));
#22348=CARTESIAN_POINT('Origin',(0.,-0.35718,0.));
#22349=CARTESIAN_POINT('Origin',(0.,-0.05953,0.));
#22350=CARTESIAN_POINT('',(0.,0.,0.));
#22351=CARTESIAN_POINT('Origin',(1.119765,0.495,0.));
#22352=CARTESIAN_POINT('',(-1.119765,0.495,-1.37131662304724E-16));
#22353=CARTESIAN_POINT('Origin',(0.,0.495,0.));
#22354=CARTESIAN_POINT('',(-1.085235,0.495,-1.32902956907268E-16));
#22355=CARTESIAN_POINT('Origin',(0.,0.495,0.));
#22356=CARTESIAN_POINT('Origin',(0.,0.4575,0.));
#22357=CARTESIAN_POINT('',(-1.119765,0.42,-1.37131662304724E-16));
#22358=CARTESIAN_POINT('Origin',(0.,0.42,0.));
#22359=CARTESIAN_POINT('',(-1.119765,0.4575,-1.37131662304724E-16));
#22360=CARTESIAN_POINT('Origin',(1.085235,0.42,0.));
#22361=CARTESIAN_POINT('',(-1.085235,0.42,-1.32902956907268E-16));
#22362=CARTESIAN_POINT('Origin',(0.,0.42,0.));
#22363=CARTESIAN_POINT('Origin',(0.,0.4575,0.));
#22364=CARTESIAN_POINT('',(-1.085235,0.4575,-1.32902956907268E-16));
#22365=CARTESIAN_POINT('Origin',(1.119765,-0.42,0.));
#22366=CARTESIAN_POINT('',(-1.119765,-0.42,-1.37131662304724E-16));
#22367=CARTESIAN_POINT('Origin',(0.,-0.42,0.));
#22368=CARTESIAN_POINT('',(-1.085235,-0.42,-1.32902956907268E-16));
#22369=CARTESIAN_POINT('Origin',(0.,-0.42,0.));
#22370=CARTESIAN_POINT('Origin',(0.,-0.4575,0.));
#22371=CARTESIAN_POINT('',(-1.119765,-0.495,-1.37131662304724E-16));
#22372=CARTESIAN_POINT('Origin',(0.,-0.495,0.));
#22373=CARTESIAN_POINT('',(-1.119765,-0.4575,-1.37131662304724E-16));
#22374=CARTESIAN_POINT('Origin',(1.085235,-0.495,0.));
#22375=CARTESIAN_POINT('',(-1.085235,-0.495,-1.32902956907268E-16));
#22376=CARTESIAN_POINT('Origin',(0.,-0.495,0.));
#22377=CARTESIAN_POINT('Origin',(0.,-0.4575,0.));
#22378=CARTESIAN_POINT('',(-1.085235,-0.4575,-1.32902956907268E-16));
#22379=CARTESIAN_POINT('',(0.,0.,0.));
#22380=CARTESIAN_POINT('',(0.,0.,0.));
#22381=CARTESIAN_POINT('',(0.,0.,0.));
#22382=CARTESIAN_POINT('',(0.,0.,0.));
#22383=CARTESIAN_POINT('',(0.,0.,0.));
#22384=CARTESIAN_POINT('',(0.,0.,0.));
#22385=CARTESIAN_POINT('',(0.,0.,0.));
#22386=CARTESIAN_POINT('',(0.,0.,0.));
#22387=CARTESIAN_POINT('',(0.,0.,0.));
#22388=CARTESIAN_POINT('',(0.,0.,0.));
#22389=CARTESIAN_POINT('',(0.,0.,0.));
#22390=CARTESIAN_POINT('',(0.,0.,0.));
#22391=CARTESIAN_POINT('',(0.,0.,0.));
#22392=CARTESIAN_POINT('',(0.,0.,0.));
#22393=CARTESIAN_POINT('',(0.,0.,0.));
#22394=CARTESIAN_POINT('',(0.,0.,0.));
#22395=CARTESIAN_POINT('',(0.,0.,0.));
#22396=CARTESIAN_POINT('',(0.,0.,0.));
#22397=CARTESIAN_POINT('',(0.,0.,0.));
#22398=CARTESIAN_POINT('',(0.,0.,0.));
#22399=CARTESIAN_POINT('',(0.,0.,0.));
#22400=CARTESIAN_POINT('',(0.,0.,0.));
#22401=CARTESIAN_POINT('',(0.,0.,0.));
#22402=CARTESIAN_POINT('',(0.,0.,0.));
#22403=CARTESIAN_POINT('',(0.,0.,0.));
#22404=CARTESIAN_POINT('',(0.,0.,0.));
#22405=CARTESIAN_POINT('',(0.,0.,15.));
#22406=CARTESIAN_POINT('',(9.39692620785909,0.,18.4202014332567));
#22407=CARTESIAN_POINT('',(0.,0.,0.));
#22408=CARTESIAN_POINT('',(0.,0.,0.));
#22409=CARTESIAN_POINT('',(0.,0.,0.));
#22410=CARTESIAN_POINT('',(0.,0.,0.));
#22411=CARTESIAN_POINT('',(0.,0.,0.));
#22412=CARTESIAN_POINT('',(0.,0.,0.));
#22413=CARTESIAN_POINT('',(0.,0.,0.));
#22414=CARTESIAN_POINT('',(0.,0.,0.));
#22415=CARTESIAN_POINT('',(0.,0.,0.));
#22416=CARTESIAN_POINT('',(0.,0.,0.));
#22417=CARTESIAN_POINT('',(0.,0.,0.));
#22418=CARTESIAN_POINT('',(0.,0.,0.));
#22419=CARTESIAN_POINT('',(0.,0.,0.));
#22420=CARTESIAN_POINT('',(0.,0.,0.));
#22421=CARTESIAN_POINT('',(0.,0.,0.));
#22422=CARTESIAN_POINT('',(0.,0.,0.));
#22423=CARTESIAN_POINT('',(0.,0.,0.));
#22424=CARTESIAN_POINT('',(0.,0.,0.));
#22425=CARTESIAN_POINT('',(0.,0.,0.));
#22426=CARTESIAN_POINT('',(0.,0.,0.));
#22427=CARTESIAN_POINT('',(0.,0.,0.));
#22428=CARTESIAN_POINT('',(18.,0.,15.));
#22429=CARTESIAN_POINT('',(24.2020784790221,0.,28.6577532024872));
#22430=CARTESIAN_POINT('',(0.,0.,0.));
#22431=CARTESIAN_POINT('',(0.,0.,0.));
#22432=CARTESIAN_POINT('Origin',(25.3520784790221,2.4,28.6577532024872));
#22433=CARTESIAN_POINT('',(25.1870784790221,2.5,28.6577532024872));
#22434=CARTESIAN_POINT('Origin',(25.3520784790221,2.5,28.6577532024872));
#22435=CARTESIAN_POINT('',(25.1870784790221,3.5,28.6577532024872));
#22436=CARTESIAN_POINT('',(25.1870784790221,2.4,28.6577532024872));
#22437=CARTESIAN_POINT('Origin',(25.3520784790221,3.5,28.6577532024872));
#22438=CARTESIAN_POINT('Origin',(23.6270784790221,2.4,29.6536824168393));
#22439=CARTESIAN_POINT('',(23.4620784790221,2.5,29.6536824168393));
#22440=CARTESIAN_POINT('Origin',(23.6270784790221,2.5,29.6536824168393));
#22441=CARTESIAN_POINT('',(23.4620784790221,3.5,29.6536824168393));
#22442=CARTESIAN_POINT('',(23.4620784790221,2.4,29.6536824168393));
#22443=CARTESIAN_POINT('Origin',(23.6270784790221,3.5,29.6536824168393));
#22444=CARTESIAN_POINT('Origin',(23.6270784790221,2.4,27.6618239881351));
#22445=CARTESIAN_POINT('',(23.4620784790221,2.5,27.6618239881351));
#22446=CARTESIAN_POINT('Origin',(23.6270784790221,2.5,27.6618239881351));
#22447=CARTESIAN_POINT('',(23.4620784790221,3.5,27.6618239881351));
#22448=CARTESIAN_POINT('',(23.4620784790221,2.4,27.6618239881351));
#22449=CARTESIAN_POINT('Origin',(23.6270784790221,3.5,27.6618239881351));
#22450=CARTESIAN_POINT('Origin',(24.2020784790221,2.4,28.6577532024872));
#22451=CARTESIAN_POINT('',(23.5970784790221,2.5,28.6577532024872));
#22452=CARTESIAN_POINT('Origin',(24.2020784790221,2.5,28.6577532024872));
#22453=CARTESIAN_POINT('',(23.5970784790221,3.5,28.6577532024872));
#22454=CARTESIAN_POINT('',(23.5970784790221,2.4,28.6577532024872));
#22455=CARTESIAN_POINT('Origin',(24.2020784790221,3.5,28.6577532024872));
#22456=CARTESIAN_POINT('Origin',(10.5469262078591,2.4,18.4202014332567));
#22457=CARTESIAN_POINT('',(10.3819262078591,2.5,18.4202014332567));
#22458=CARTESIAN_POINT('Origin',(10.5469262078591,2.5,18.4202014332567));
#22459=CARTESIAN_POINT('',(10.3819262078591,3.5,18.4202014332567));
#22460=CARTESIAN_POINT('',(10.3819262078591,2.4,18.4202014332567));
#22461=CARTESIAN_POINT('Origin',(10.5469262078591,3.5,18.4202014332567));
#22462=CARTESIAN_POINT('Origin',(8.82192620785908,2.4,19.4161306476088));
#22463=CARTESIAN_POINT('',(8.65692620785908,2.5,19.4161306476088));
#22464=CARTESIAN_POINT('Origin',(8.82192620785908,2.5,19.4161306476088));
#22465=CARTESIAN_POINT('',(8.65692620785908,3.5,19.4161306476088));
#22466=CARTESIAN_POINT('',(8.65692620785908,2.4,19.4161306476088));
#22467=CARTESIAN_POINT('Origin',(8.82192620785908,3.5,19.4161306476088));
#22468=CARTESIAN_POINT('Origin',(8.82192620785908,2.4,17.4242722189046));
#22469=CARTESIAN_POINT('',(8.65692620785908,2.5,17.4242722189046));
#22470=CARTESIAN_POINT('Origin',(8.82192620785908,2.5,17.4242722189046));
#22471=CARTESIAN_POINT('',(8.65692620785908,3.5,17.4242722189046));
#22472=CARTESIAN_POINT('',(8.65692620785908,2.4,17.4242722189046));
#22473=CARTESIAN_POINT('Origin',(8.82192620785908,3.5,17.4242722189046));
#22474=CARTESIAN_POINT('Origin',(9.39692620785909,2.4,18.4202014332567));
#22475=CARTESIAN_POINT('',(8.79192620785908,2.5,18.4202014332567));
#22476=CARTESIAN_POINT('Origin',(9.39692620785909,2.5,18.4202014332567));
#22477=CARTESIAN_POINT('',(8.79192620785908,3.5,18.4202014332567));
#22478=CARTESIAN_POINT('',(8.79192620785908,2.4,18.4202014332567));
#22479=CARTESIAN_POINT('Origin',(9.39692620785909,3.5,18.4202014332567));
#22480=CARTESIAN_POINT('Origin',(23.0020784790221,2.5,28.6577532024872));
#22481=CARTESIAN_POINT('',(23.0020784790221,2.5,29.9993939889871));
#22482=CARTESIAN_POINT('',(23.0020784790221,3.5,29.9993939889871));
#22483=CARTESIAN_POINT('',(23.0020784790221,2.5,29.9993939889871));
#22484=CARTESIAN_POINT('',(23.0020784790221,2.5,32.));
#22485=CARTESIAN_POINT('',(23.0020784790221,2.5,32.));
#22486=CARTESIAN_POINT('',(23.0020784790221,3.5,32.));
#22487=CARTESIAN_POINT('',(23.0020784790221,2.5,32.));
#22488=CARTESIAN_POINT('',(23.0020784790221,3.5,32.));
#22489=CARTESIAN_POINT('Origin',(25.4020784790221,2.5,32.));
#22490=CARTESIAN_POINT('',(25.4020784790221,3.5,29.9993939889871));
#22491=CARTESIAN_POINT('',(25.4020784790221,2.5,29.9993939889871));
#22492=CARTESIAN_POINT('',(25.4020784790221,2.5,29.9993939889871));
#22493=CARTESIAN_POINT('',(25.4020784790221,3.5,32.));
#22494=CARTESIAN_POINT('',(25.4020784790221,3.5,28.6577532024872));
#22495=CARTESIAN_POINT('',(25.4020784790221,2.5,32.));
#22496=CARTESIAN_POINT('',(25.4020784790221,2.5,32.));
#22497=CARTESIAN_POINT('',(25.4020784790221,2.5,28.6577532024872));
#22498=CARTESIAN_POINT('Origin',(23.0020784790221,2.5,32.));
#22499=CARTESIAN_POINT('',(25.4020784790221,2.5,32.));
#22500=CARTESIAN_POINT('',(25.4020784790221,3.5,32.));
#22501=CARTESIAN_POINT('Origin',(24.2020784790221,2.5,28.6577532024872));
#22502=CARTESIAN_POINT('',(22.4045561490901,3.5,28.7521643956565));
#22503=CARTESIAN_POINT('Origin',(24.2020784790221,3.5,28.6577532024872));
#22504=CARTESIAN_POINT('',(22.4045561490901,2.5,28.7521643956565));
#22505=CARTESIAN_POINT('',(22.4045561490901,2.5,28.7521643956565));
#22506=CARTESIAN_POINT('Origin',(24.2020784790221,2.5,28.6577532024872));
#22507=CARTESIAN_POINT('Origin',(24.2020784790221,2.5,28.6577532024872));
#22508=CARTESIAN_POINT('',(23.6558124764405,2.5,26.9426457847365));
#22509=CARTESIAN_POINT('Origin',(24.2020784790221,2.5,28.6577532024872));
#22510=CARTESIAN_POINT('',(23.6558124764405,3.5,26.9426457847365));
#22511=CARTESIAN_POINT('',(23.6558124764405,2.5,26.9426457847365));
#22512=CARTESIAN_POINT('Origin',(24.2020784790221,3.5,28.6577532024872));
#22513=CARTESIAN_POINT('Origin',(16.7995023434406,2.5,23.538977317872));
#22514=CARTESIAN_POINT('',(10.5969262078591,2.5,20.5873565921787));
#22515=CARTESIAN_POINT('',(8.77129804418388,2.5,19.3249607387167));
#22516=CARTESIAN_POINT('',(10.5969262078591,2.5,32.));
#22517=CARTESIAN_POINT('',(10.5969262078591,2.5,18.4202014332567));
#22518=CARTESIAN_POINT('',(8.19692620785908,2.5,32.));
#22519=CARTESIAN_POINT('',(10.5969262078591,2.5,32.));
#22520=CARTESIAN_POINT('',(8.19692620785908,2.5,19.7618422197566));
#22521=CARTESIAN_POINT('',(8.19692620785908,2.5,32.));
#22522=CARTESIAN_POINT('',(11.1944485377911,2.5,18.3257902400875));
#22523=CARTESIAN_POINT('Origin',(9.39692620785909,2.5,18.4202014332567));
#22524=CARTESIAN_POINT('',(24.8277066426973,2.5,27.7529938970273));
#22525=CARTESIAN_POINT('Origin',(8.19692620785908,2.5,18.4202014332567));
#22526=CARTESIAN_POINT('',(8.19692620785908,3.5,19.7618422197566));
#22527=CARTESIAN_POINT('',(8.19692620785908,2.5,19.7618422197566));
#22528=CARTESIAN_POINT('',(8.19692620785908,3.5,32.));
#22529=CARTESIAN_POINT('',(8.19692620785908,2.5,32.));
#22530=CARTESIAN_POINT('',(8.19692620785908,3.5,32.));
#22531=CARTESIAN_POINT('Origin',(10.5969262078591,2.5,32.));
#22532=CARTESIAN_POINT('',(10.5969262078591,3.5,20.5873565921787));
#22533=CARTESIAN_POINT('',(10.5969262078591,2.5,20.5873565921787));
#22534=CARTESIAN_POINT('',(10.5969262078591,3.5,32.));
#22535=CARTESIAN_POINT('',(10.5969262078591,3.5,18.4202014332567));
#22536=CARTESIAN_POINT('',(10.5969262078591,2.5,32.));
#22537=CARTESIAN_POINT('Origin',(8.19692620785908,2.5,32.));
#22538=CARTESIAN_POINT('',(10.5969262078591,3.5,32.));
#22539=CARTESIAN_POINT('Origin',(8.77129804418388,2.5,19.3249607387167));
#22540=CARTESIAN_POINT('',(8.77129804418388,3.5,19.3249607387167));
#22541=CARTESIAN_POINT('Origin',(9.39692620785909,2.5,18.4202014332567));
#22542=CARTESIAN_POINT('',(11.1944485377911,3.5,18.3257902400875));
#22543=CARTESIAN_POINT('Origin',(9.39692620785909,3.5,18.4202014332567));
#22544=CARTESIAN_POINT('',(11.1944485377911,2.5,18.3257902400875));
#22545=CARTESIAN_POINT('Origin',(24.8277066426973,2.5,27.7529938970273));
#22546=CARTESIAN_POINT('',(24.8277066426973,3.5,27.7529938970273));
#22547=CARTESIAN_POINT('Origin',(16.7995023434406,3.5,23.538977317872));
#22548=CARTESIAN_POINT('Origin',(28.,7.5,32.));
#22549=CARTESIAN_POINT('',(28.,7.5,32.));
#22550=CARTESIAN_POINT('',(8.,7.5,32.));
#22551=CARTESIAN_POINT('',(28.,7.5,32.));
#22552=CARTESIAN_POINT('',(8.,7.5,32.8));
#22553=CARTESIAN_POINT('',(8.,7.5,32.));
#22554=CARTESIAN_POINT('',(28.,7.5,32.8));
#22555=CARTESIAN_POINT('',(28.,7.5,32.8));
#22556=CARTESIAN_POINT('',(28.,7.5,32.));
#22557=CARTESIAN_POINT('Origin',(28.,-3.5,32.));
#22558=CARTESIAN_POINT('',(28.,-3.5,32.));
#22559=CARTESIAN_POINT('',(28.,-3.5,32.));
#22560=CARTESIAN_POINT('',(28.,-3.5,32.8));
#22561=CARTESIAN_POINT('',(28.,-3.5,32.8));
#22562=CARTESIAN_POINT('',(28.,-3.5,32.));
#22563=CARTESIAN_POINT('Origin',(8.,-3.5,32.));
#22564=CARTESIAN_POINT('',(8.,-3.5,32.));
#22565=CARTESIAN_POINT('',(8.,-3.5,32.));
#22566=CARTESIAN_POINT('',(8.,-3.5,32.8));
#22567=CARTESIAN_POINT('',(8.,-3.5,32.8));
#22568=CARTESIAN_POINT('',(8.,-3.5,32.));
#22569=CARTESIAN_POINT('Origin',(8.,7.5,32.));
#22570=CARTESIAN_POINT('',(8.,7.5,32.));
#22571=CARTESIAN_POINT('',(8.,7.5,32.8));
#22572=CARTESIAN_POINT('Origin',(18.,2.,32.8));
#22573=CARTESIAN_POINT('Origin',(18.,2.,32.));
#22574=CARTESIAN_POINT('',(0.,0.,0.));
#22575=CARTESIAN_POINT('Origin',(8.8,7.5,32.8));
#22576=CARTESIAN_POINT('',(8.8,7.5,32.8));
#22577=CARTESIAN_POINT('',(8.,7.5,32.8));
#22578=CARTESIAN_POINT('',(8.8,7.5,32.8));
#22579=CARTESIAN_POINT('',(8.,7.5,35.3));
#22580=CARTESIAN_POINT('',(8.,7.5,32.8));
#22581=CARTESIAN_POINT('',(8.8,7.5,35.3));
#22582=CARTESIAN_POINT('',(8.8,7.5,35.3));
#22583=CARTESIAN_POINT('',(8.8,7.5,32.8));
#22584=CARTESIAN_POINT('Origin',(8.8,-3.5,32.8));
#22585=CARTESIAN_POINT('',(8.8,-3.5,32.8));
#22586=CARTESIAN_POINT('',(8.8,-3.5,32.8));
#22587=CARTESIAN_POINT('',(8.8,-3.5,35.3));
#22588=CARTESIAN_POINT('',(8.8,-3.5,35.3));
#22589=CARTESIAN_POINT('',(8.8,-3.5,32.8));
#22590=CARTESIAN_POINT('Origin',(8.,-3.5,32.8));
#22591=CARTESIAN_POINT('',(8.,-3.5,32.8));
#22592=CARTESIAN_POINT('',(8.,-3.5,32.8));
#22593=CARTESIAN_POINT('',(8.,-3.5,35.3));
#22594=CARTESIAN_POINT('',(8.,-3.5,35.3));
#22595=CARTESIAN_POINT('',(8.,-3.5,32.8));
#22596=CARTESIAN_POINT('Origin',(8.,7.5,32.8));
#22597=CARTESIAN_POINT('',(8.,7.5,32.8));
#22598=CARTESIAN_POINT('',(8.,7.5,35.3));
#22599=CARTESIAN_POINT('Origin',(8.4,2.,35.3));
#22600=CARTESIAN_POINT('Origin',(8.4,2.,32.8));
#22601=CARTESIAN_POINT('',(0.,0.,0.));
#22602=CARTESIAN_POINT('Origin',(28.,7.5,32.8));
#22603=CARTESIAN_POINT('',(28.,7.5,32.8));
#22604=CARTESIAN_POINT('',(27.2,7.5,32.8));
#22605=CARTESIAN_POINT('',(28.,7.5,32.8));
#22606=CARTESIAN_POINT('',(27.2,7.5,35.3));
#22607=CARTESIAN_POINT('',(27.2,7.5,32.8));
#22608=CARTESIAN_POINT('',(28.,7.5,35.3));
#22609=CARTESIAN_POINT('',(28.,7.5,35.3));
#22610=CARTESIAN_POINT('',(28.,7.5,32.8));
#22611=CARTESIAN_POINT('Origin',(28.,-3.5,32.8));
#22612=CARTESIAN_POINT('',(28.,-3.5,32.8));
#22613=CARTESIAN_POINT('',(28.,-3.5,32.8));
#22614=CARTESIAN_POINT('',(28.,-3.5,35.3));
#22615=CARTESIAN_POINT('',(28.,-3.5,35.3));
#22616=CARTESIAN_POINT('',(28.,-3.5,32.8));
#22617=CARTESIAN_POINT('Origin',(27.2,-3.5,32.8));
#22618=CARTESIAN_POINT('',(27.2,-3.5,32.8));
#22619=CARTESIAN_POINT('',(27.2,-3.5,32.8));
#22620=CARTESIAN_POINT('',(27.2,-3.5,35.3));
#22621=CARTESIAN_POINT('',(27.2,-3.5,35.3));
#22622=CARTESIAN_POINT('',(27.2,-3.5,32.8));
#22623=CARTESIAN_POINT('Origin',(27.2,7.5,32.8));
#22624=CARTESIAN_POINT('',(27.2,7.5,32.8));
#22625=CARTESIAN_POINT('',(27.2,7.5,35.3));
#22626=CARTESIAN_POINT('Origin',(27.6,2.,35.3));
#22627=CARTESIAN_POINT('Origin',(27.6,2.,32.8));
#22628=CARTESIAN_POINT('',(0.,0.,0.));
#22629=CARTESIAN_POINT('Origin',(9.39692620785909,-5.6,18.4202014332567));
#22630=CARTESIAN_POINT('',(9.23192620785909,-5.5,18.4202014332567));
#22631=CARTESIAN_POINT('Origin',(9.39692620785909,-5.5,18.4202014332567));
#22632=CARTESIAN_POINT('',(9.23192620785909,-3.9,18.4202014332567));
#22633=CARTESIAN_POINT('',(9.23192620785909,-5.6,18.4202014332567));
#22634=CARTESIAN_POINT('Origin',(9.39692620785909,-3.9,18.4202014332567));
#22635=CARTESIAN_POINT('Origin',(9.39692620785909,-3.9,18.4202014332567));
#22636=CARTESIAN_POINT('Origin',(10.5469262078591,2.,18.4202014332567));
#22637=CARTESIAN_POINT('',(10.3219262078591,2.1,18.4202014332567));
#22638=CARTESIAN_POINT('Origin',(10.5469262078591,2.1,18.4202014332567));
#22639=CARTESIAN_POINT('',(10.3219262078591,2.5,18.4202014332567));
#22640=CARTESIAN_POINT('',(10.3219262078591,2.,18.4202014332567));
#22641=CARTESIAN_POINT('Origin',(10.5469262078591,2.5,18.4202014332567));
#22642=CARTESIAN_POINT('Origin',(8.82192620785908,2.,19.4161306476088));
#22643=CARTESIAN_POINT('',(8.59692620785908,2.1,19.4161306476088));
#22644=CARTESIAN_POINT('Origin',(8.82192620785908,2.1,19.4161306476088));
#22645=CARTESIAN_POINT('',(8.59692620785908,2.5,19.4161306476088));
#22646=CARTESIAN_POINT('',(8.59692620785908,2.,19.4161306476088));
#22647=CARTESIAN_POINT('Origin',(8.82192620785908,2.5,19.4161306476088));
#22648=CARTESIAN_POINT('Origin',(8.82192620785908,2.,17.4242722189046));
#22649=CARTESIAN_POINT('',(8.59692620785908,2.1,17.4242722189046));
#22650=CARTESIAN_POINT('Origin',(8.82192620785908,2.1,17.4242722189046));
#22651=CARTESIAN_POINT('',(8.59692620785908,2.5,17.4242722189046));
#22652=CARTESIAN_POINT('',(8.59692620785908,2.,17.4242722189046));
#22653=CARTESIAN_POINT('Origin',(8.82192620785908,2.5,17.4242722189046));
#22654=CARTESIAN_POINT('Origin',(9.39692620785909,2.5,18.4202014332567));
#22655=CARTESIAN_POINT('',(7.89692620785909,2.5,18.4202014332567));
#22656=CARTESIAN_POINT('Origin',(9.39692620785909,2.5,18.4202014332567));
#22657=CARTESIAN_POINT('',(8.79692620785909,2.5,18.4202014332567));
#22658=CARTESIAN_POINT('Origin',(9.39692620785909,2.5,18.4202014332567));
#22659=CARTESIAN_POINT('Origin',(9.39692620785909,2.1,18.4202014332567));
#22660=CARTESIAN_POINT('',(7.89692620785909,2.1,18.4202014332567));
#22661=CARTESIAN_POINT('Origin',(9.39692620785909,2.1,18.4202014332567));
#22662=CARTESIAN_POINT('',(8.79692620785909,2.1,18.4202014332567));
#22663=CARTESIAN_POINT('Origin',(9.39692620785909,2.1,18.4202014332567));
#22664=CARTESIAN_POINT('Origin',(9.39692620785909,2.1,18.4202014332567));
#22665=CARTESIAN_POINT('',(7.89692620785909,2.1,18.4202014332567));
#22666=CARTESIAN_POINT('Origin',(9.39692620785909,-5.5,18.4202014332567));
#22667=CARTESIAN_POINT('',(8.79692620785909,-5.5,18.4202014332567));
#22668=CARTESIAN_POINT('',(8.79692620785909,-5.5,18.4202014332567));
#22669=CARTESIAN_POINT('Origin',(9.39692620785909,-5.5,18.4202014332567));
#22670=CARTESIAN_POINT('Origin',(9.39692620785909,-5.5,18.4202014332567));
#22671=CARTESIAN_POINT('',(8.79692620785909,3.5,18.4202014332567));
#22672=CARTESIAN_POINT('Origin',(9.39692620785909,3.5,18.4202014332567));
#22673=CARTESIAN_POINT('',(8.79692620785909,-5.5,18.4202014332567));
#22674=CARTESIAN_POINT('Origin',(9.39692620785909,3.5,18.4202014332567));
#22675=CARTESIAN_POINT('Origin',(9.39692620785909,-5.5,18.4202014332567));
#22676=CARTESIAN_POINT('',(0.,0.,0.));
#22677=CARTESIAN_POINT('Origin',(9.39692620785909,0.5,18.4202014332567));
#22678=CARTESIAN_POINT('',(8.79192620785908,2.1,18.4202014332567));
#22679=CARTESIAN_POINT('Origin',(9.39692620785909,2.1,18.4202014332567));
#22680=CARTESIAN_POINT('',(8.79192620785908,0.5,18.4202014332567));
#22681=CARTESIAN_POINT('',(8.79192620785908,0.5,18.4202014332567));
#22682=CARTESIAN_POINT('Origin',(9.39692620785909,0.5,18.4202014332567));
#22683=CARTESIAN_POINT('Origin',(9.39692620785909,0.5,18.4202014332567));
#22684=CARTESIAN_POINT('',(8.59692620785908,2.1,18.4202014332567));
#22685=CARTESIAN_POINT('Origin',(9.39692620785909,2.1,18.4202014332567));
#22686=CARTESIAN_POINT('',(8.59692620785908,0.5,18.4202014332567));
#22687=CARTESIAN_POINT('',(8.59692620785908,0.5,18.4202014332567));
#22688=CARTESIAN_POINT('Origin',(9.39692620785909,0.5,18.4202014332567));
#22689=CARTESIAN_POINT('Origin',(9.39692620785909,2.1,18.4202014332567));
#22690=CARTESIAN_POINT('Origin',(9.39692620785909,0.5,18.4202014332567));
#22691=CARTESIAN_POINT('',(0.,0.,0.));
#22692=CARTESIAN_POINT('Origin',(9.39692620785909,-4.,18.4202014332567));
#22693=CARTESIAN_POINT('',(8.79192620785908,-0.5,18.4202014332567));
#22694=CARTESIAN_POINT('Origin',(9.39692620785909,-0.5,18.4202014332567));
#22695=CARTESIAN_POINT('',(8.79192620785908,-4.,18.4202014332567));
#22696=CARTESIAN_POINT('',(8.79192620785908,-4.,18.4202014332567));
#22697=CARTESIAN_POINT('Origin',(9.39692620785909,-4.,18.4202014332567));
#22698=CARTESIAN_POINT('Origin',(9.39692620785909,-4.,18.4202014332567));
#22699=CARTESIAN_POINT('',(8.59692620785908,-0.5,18.4202014332567));
#22700=CARTESIAN_POINT('Origin',(9.39692620785909,-0.5,18.4202014332567));
#22701=CARTESIAN_POINT('',(8.59692620785908,-4.,18.4202014332567));
#22702=CARTESIAN_POINT('',(8.59692620785908,-4.,18.4202014332567));
#22703=CARTESIAN_POINT('Origin',(9.39692620785909,-4.,18.4202014332567));
#22704=CARTESIAN_POINT('Origin',(9.39692620785909,-0.5,18.4202014332567));
#22705=CARTESIAN_POINT('Origin',(9.39692620785909,-4.,18.4202014332567));
#22706=CARTESIAN_POINT('',(0.,0.,0.));
#22707=CARTESIAN_POINT('Origin',(9.39692620785909,-5.5,18.4202014332567));
#22708=CARTESIAN_POINT('',(8.79192620785908,-5.,18.4202014332567));
#22709=CARTESIAN_POINT('Origin',(9.39692620785909,-5.,18.4202014332567));
#22710=CARTESIAN_POINT('',(8.79192620785908,-5.5,18.4202014332567));
#22711=CARTESIAN_POINT('',(8.79192620785908,-5.5,18.4202014332567));
#22712=CARTESIAN_POINT('Origin',(9.39692620785909,-5.5,18.4202014332567));
#22713=CARTESIAN_POINT('Origin',(9.39692620785909,-5.5,18.4202014332567));
#22714=CARTESIAN_POINT('',(8.59692620785908,-5.,18.4202014332567));
#22715=CARTESIAN_POINT('Origin',(9.39692620785909,-5.,18.4202014332567));
#22716=CARTESIAN_POINT('',(8.59692620785908,-5.5,18.4202014332567));
#22717=CARTESIAN_POINT('',(8.59692620785908,-5.5,18.4202014332567));
#22718=CARTESIAN_POINT('Origin',(9.39692620785909,-5.5,18.4202014332567));
#22719=CARTESIAN_POINT('Origin',(9.39692620785909,-5.,18.4202014332567));
#22720=CARTESIAN_POINT('Origin',(9.39692620785909,-5.5,18.4202014332567));
#22721=CARTESIAN_POINT('',(0.,0.,0.));
#22722=CARTESIAN_POINT('Origin',(9.39692620785909,-5.7,18.4202014332567));
#22723=CARTESIAN_POINT('',(9.17192620785909,-5.5,18.4202014332567));
#22724=CARTESIAN_POINT('Origin',(9.39692620785909,-5.5,18.4202014332567));
#22725=CARTESIAN_POINT('',(9.17192620785909,-5.7,18.4202014332567));
#22726=CARTESIAN_POINT('',(9.17192620785909,-5.7,18.4202014332567));
#22727=CARTESIAN_POINT('Origin',(9.39692620785909,-5.7,18.4202014332567));
#22728=CARTESIAN_POINT('Origin',(9.39692620785909,-5.7,18.4202014332567));
#22729=CARTESIAN_POINT('',(8.39692620785909,-5.5,18.4202014332567));
#22730=CARTESIAN_POINT('Origin',(9.39692620785909,-5.5,18.4202014332567));
#22731=CARTESIAN_POINT('',(8.39692620785909,-5.7,18.4202014332567));
#22732=CARTESIAN_POINT('',(8.39692620785909,-5.7,18.4202014332567));
#22733=CARTESIAN_POINT('Origin',(9.39692620785909,-5.7,18.4202014332567));
#22734=CARTESIAN_POINT('Origin',(9.39692620785909,-5.5,18.4202014332567));
#22735=CARTESIAN_POINT('Origin',(9.39692620785909,-5.7,18.4202014332567));
#22736=CARTESIAN_POINT('',(0.,0.,0.));
#22737=CARTESIAN_POINT('Origin',(24.2020784790221,-1.1,28.6577532024872));
#22738=CARTESIAN_POINT('',(24.0370784790221,-1.,28.6577532024872));
#22739=CARTESIAN_POINT('Origin',(24.2020784790221,-1.,28.6577532024872));
#22740=CARTESIAN_POINT('',(24.0370784790221,0.6,28.6577532024872));
#22741=CARTESIAN_POINT('',(24.0370784790221,-1.1,28.6577532024872));
#22742=CARTESIAN_POINT('Origin',(24.2020784790221,0.6,28.6577532024872));
#22743=CARTESIAN_POINT('Origin',(24.2020784790221,0.6,28.6577532024872));
#22744=CARTESIAN_POINT('Origin',(25.3520784790221,2.,28.6577532024872));
#22745=CARTESIAN_POINT('',(25.1270784790221,2.1,28.6577532024872));
#22746=CARTESIAN_POINT('Origin',(25.3520784790221,2.1,28.6577532024872));
#22747=CARTESIAN_POINT('',(25.1270784790221,2.5,28.6577532024872));
#22748=CARTESIAN_POINT('',(25.1270784790221,2.,28.6577532024872));
#22749=CARTESIAN_POINT('Origin',(25.3520784790221,2.5,28.6577532024872));
#22750=CARTESIAN_POINT('Origin',(23.6270784790221,2.,29.6536824168393));
#22751=CARTESIAN_POINT('',(23.4020784790221,2.1,29.6536824168393));
#22752=CARTESIAN_POINT('Origin',(23.6270784790221,2.1,29.6536824168393));
#22753=CARTESIAN_POINT('',(23.4020784790221,2.5,29.6536824168393));
#22754=CARTESIAN_POINT('',(23.4020784790221,2.,29.6536824168393));
#22755=CARTESIAN_POINT('Origin',(23.6270784790221,2.5,29.6536824168393));
#22756=CARTESIAN_POINT('Origin',(23.6270784790221,2.,27.6618239881351));
#22757=CARTESIAN_POINT('',(23.4020784790221,2.1,27.6618239881351));
#22758=CARTESIAN_POINT('Origin',(23.6270784790221,2.1,27.6618239881351));
#22759=CARTESIAN_POINT('',(23.4020784790221,2.5,27.6618239881351));
#22760=CARTESIAN_POINT('',(23.4020784790221,2.,27.6618239881351));
#22761=CARTESIAN_POINT('Origin',(23.6270784790221,2.5,27.6618239881351));
#22762=CARTESIAN_POINT('Origin',(24.2020784790221,2.5,28.6577532024872));
#22763=CARTESIAN_POINT('',(22.7020784790221,2.5,28.6577532024872));
#22764=CARTESIAN_POINT('Origin',(24.2020784790221,2.5,28.6577532024872));
#22765=CARTESIAN_POINT('',(23.6020784790221,2.5,28.6577532024872));
#22766=CARTESIAN_POINT('Origin',(24.2020784790221,2.5,28.6577532024872));
#22767=CARTESIAN_POINT('Origin',(24.2020784790221,2.1,28.6577532024872));
#22768=CARTESIAN_POINT('',(22.7020784790221,2.1,28.6577532024872));
#22769=CARTESIAN_POINT('Origin',(24.2020784790221,2.1,28.6577532024872));
#22770=CARTESIAN_POINT('',(23.6020784790221,2.1,28.6577532024872));
#22771=CARTESIAN_POINT('Origin',(24.2020784790221,2.1,28.6577532024872));
#22772=CARTESIAN_POINT('Origin',(24.2020784790221,2.1,28.6577532024872));
#22773=CARTESIAN_POINT('',(22.7020784790221,2.1,28.6577532024872));
#22774=CARTESIAN_POINT('Origin',(24.2020784790221,-1.,28.6577532024872));
#22775=CARTESIAN_POINT('',(23.6020784790221,-1.,28.6577532024872));
#22776=CARTESIAN_POINT('',(23.6020784790221,-1.,28.6577532024872));
#22777=CARTESIAN_POINT('Origin',(24.2020784790221,-1.,28.6577532024872));
#22778=CARTESIAN_POINT('Origin',(24.2020784790221,-1.,28.6577532024872));
#22779=CARTESIAN_POINT('',(23.6020784790221,3.5,28.6577532024872));
#22780=CARTESIAN_POINT('Origin',(24.2020784790221,3.5,28.6577532024872));
#22781=CARTESIAN_POINT('',(23.6020784790221,-1.,28.6577532024872));
#22782=CARTESIAN_POINT('Origin',(24.2020784790221,3.5,28.6577532024872));
#22783=CARTESIAN_POINT('Origin',(24.2020784790221,-1.,28.6577532024872));
#22784=CARTESIAN_POINT('',(0.,0.,0.));
#22785=CARTESIAN_POINT('Origin',(24.2020784790221,0.5,28.6577532024872));
#22786=CARTESIAN_POINT('',(23.5970784790221,2.1,28.6577532024872));
#22787=CARTESIAN_POINT('Origin',(24.2020784790221,2.1,28.6577532024872));
#22788=CARTESIAN_POINT('',(23.5970784790221,0.5,28.6577532024872));
#22789=CARTESIAN_POINT('',(23.5970784790221,0.5,28.6577532024872));
#22790=CARTESIAN_POINT('Origin',(24.2020784790221,0.5,28.6577532024872));
#22791=CARTESIAN_POINT('Origin',(24.2020784790221,0.5,28.6577532024872));
#22792=CARTESIAN_POINT('',(23.4020784790221,2.1,28.6577532024872));
#22793=CARTESIAN_POINT('Origin',(24.2020784790221,2.1,28.6577532024872));
#22794=CARTESIAN_POINT('',(23.4020784790221,0.5,28.6577532024872));
#22795=CARTESIAN_POINT('',(23.4020784790221,0.5,28.6577532024872));
#22796=CARTESIAN_POINT('Origin',(24.2020784790221,0.5,28.6577532024872));
#22797=CARTESIAN_POINT('Origin',(24.2020784790221,2.1,28.6577532024872));
#22798=CARTESIAN_POINT('Origin',(24.2020784790221,0.5,28.6577532024872));
#22799=CARTESIAN_POINT('',(0.,0.,0.));
#22800=CARTESIAN_POINT('Origin',(24.2020784790221,-1.,28.6577532024872));
#22801=CARTESIAN_POINT('',(23.5970784790221,-0.5,28.6577532024872));
#22802=CARTESIAN_POINT('Origin',(24.2020784790221,-0.5,28.6577532024872));
#22803=CARTESIAN_POINT('',(23.5970784790221,-1.,28.6577532024872));
#22804=CARTESIAN_POINT('',(23.5970784790221,-1.,28.6577532024872));
#22805=CARTESIAN_POINT('Origin',(24.2020784790221,-1.,28.6577532024872));
#22806=CARTESIAN_POINT('Origin',(24.2020784790221,-1.,28.6577532024872));
#22807=CARTESIAN_POINT('',(23.4020784790221,-0.5,28.6577532024872));
#22808=CARTESIAN_POINT('Origin',(24.2020784790221,-0.5,28.6577532024872));
#22809=CARTESIAN_POINT('',(23.4020784790221,-1.,28.6577532024872));
#22810=CARTESIAN_POINT('',(23.4020784790221,-1.,28.6577532024872));
#22811=CARTESIAN_POINT('Origin',(24.2020784790221,-1.,28.6577532024872));
#22812=CARTESIAN_POINT('Origin',(24.2020784790221,-0.5,28.6577532024872));
#22813=CARTESIAN_POINT('Origin',(24.2020784790221,-1.,28.6577532024872));
#22814=CARTESIAN_POINT('',(0.,0.,0.));
#22815=CARTESIAN_POINT('Origin',(24.2020784790221,-1.2,28.6577532024872));
#22816=CARTESIAN_POINT('',(23.9770784790221,-1.,28.6577532024872));
#22817=CARTESIAN_POINT('Origin',(24.2020784790221,-1.,28.6577532024872));
#22818=CARTESIAN_POINT('',(23.9770784790221,-1.2,28.6577532024872));
#22819=CARTESIAN_POINT('',(23.9770784790221,-1.2,28.6577532024872));
#22820=CARTESIAN_POINT('Origin',(24.2020784790221,-1.2,28.6577532024872));
#22821=CARTESIAN_POINT('Origin',(24.2020784790221,-1.2,28.6577532024872));
#22822=CARTESIAN_POINT('',(23.2020784790221,-1.,28.6577532024872));
#22823=CARTESIAN_POINT('Origin',(24.2020784790221,-1.,28.6577532024872));
#22824=CARTESIAN_POINT('',(23.2020784790221,-1.2,28.6577532024872));
#22825=CARTESIAN_POINT('',(23.2020784790221,-1.2,28.6577532024872));
#22826=CARTESIAN_POINT('Origin',(24.2020784790221,-1.2,28.6577532024872));
#22827=CARTESIAN_POINT('Origin',(24.2020784790221,-1.,28.6577532024872));
#22828=CARTESIAN_POINT('Origin',(24.2020784790221,-1.2,28.6577532024872));
#22829=CARTESIAN_POINT('',(0.,0.,0.));
#22830=CARTESIAN_POINT('Origin',(0.3,0.4,0.));
#22831=CARTESIAN_POINT('',(-0.3,0.4,-3.67394039744206E-17));
#22832=CARTESIAN_POINT('Origin',(0.,0.4,0.));
#22833=CARTESIAN_POINT('Origin',(0.,0.375,0.));
#22834=CARTESIAN_POINT('',(-0.35,0.35,-4.28626379701573E-17));
#22835=CARTESIAN_POINT('Origin',(0.,0.35,0.));
#22836=CARTESIAN_POINT('',(-0.325,0.375,-3.9801020972289E-17));
#22837=CARTESIAN_POINT('Origin',(0.,0.19,0.));
#22838=CARTESIAN_POINT('',(-0.35,0.03,-4.28626379701574E-17));
#22839=CARTESIAN_POINT('Origin',(0.,0.03,0.));
#22840=CARTESIAN_POINT('',(-0.35,0.19,-4.28626379701574E-17));
#22841=CARTESIAN_POINT('Origin',(0.,0.0149999999999999,0.));
#22842=CARTESIAN_POINT('',(-0.32,-3.29597460435593E-17,-3.91886975727153E-17));
#22843=CARTESIAN_POINT('Origin',(0.,0.,0.));
#22844=CARTESIAN_POINT('',(-0.335,0.0149999999999999,-4.10256677714363E-17));
#22845=CARTESIAN_POINT('Origin',(0.22,0.,0.));
#22846=CARTESIAN_POINT('',(-0.22,-6.93889390390723E-18,-2.69422295812418E-17));
#22847=CARTESIAN_POINT('Origin',(0.,0.,0.));
#22848=CARTESIAN_POINT('Origin',(0.,-0.02,0.));
#22849=CARTESIAN_POINT('',(-0.1954,-0.0492,2.39295984553393E-17));
#22850=CARTESIAN_POINT('Origin',(0.,-0.0492,0.));
#22851=CARTESIAN_POINT('',(-0.21,-0.02,-2.57175827820944E-17));
#22852=CARTESIAN_POINT('Origin',(0.,-0.8,0.));
#22853=CARTESIAN_POINT('',(-0.1954,-1.5646,2.39295984553393E-17));
#22854=CARTESIAN_POINT('Origin',(0.,-1.5646,0.));
#22855=CARTESIAN_POINT('',(-0.1954,-0.8,-2.39295984553393E-17));
#22856=CARTESIAN_POINT('Origin',(0.,-1.58,0.));
#22857=CARTESIAN_POINT('',(-0.16,-1.6,-1.95943487863577E-17));
#22858=CARTESIAN_POINT('Origin',(0.,-1.6,0.));
#22859=CARTESIAN_POINT('',(-0.18,-1.58,-2.20436423846524E-17));
#22860=CARTESIAN_POINT('Origin',(0.,-1.6,0.));
#22861=CARTESIAN_POINT('Origin',(0.0866025403784439,-0.4,-0.15));
#22862=CARTESIAN_POINT('',(0.173205080756888,-0.4,0.));
#22863=CARTESIAN_POINT('',(0.0866025403784439,-0.4,-0.15));
#22864=CARTESIAN_POINT('',(0.173205080756888,-0.4,0.));
#22865=CARTESIAN_POINT('',(0.0866025403784439,-0.64,-0.15));
#22866=CARTESIAN_POINT('',(0.0866025403784439,-0.4,-0.15));
#22867=CARTESIAN_POINT('',(0.173205080756888,-0.64,0.));
#22868=CARTESIAN_POINT('',(0.173205080756888,-0.64,0.));
#22869=CARTESIAN_POINT('',(0.173205080756888,-0.4,0.));
#22870=CARTESIAN_POINT('Origin',(-0.0866025403784438,-0.4,-0.15));
#22871=CARTESIAN_POINT('',(-0.0866025403784438,-0.4,-0.15));
#22872=CARTESIAN_POINT('',(0.0866025403784439,-0.4,-0.15));
#22873=CARTESIAN_POINT('',(-0.0866025403784438,-0.64,-0.15));
#22874=CARTESIAN_POINT('',(-0.0866025403784438,-0.4,-0.15));
#22875=CARTESIAN_POINT('',(0.0866025403784439,-0.64,-0.15));
#22876=CARTESIAN_POINT('Origin',(-0.173205080756888,-0.4,-2.77555756156289E-17));
#22877=CARTESIAN_POINT('',(-0.173205080756888,-0.4,-2.12115047744981E-17));
#22878=CARTESIAN_POINT('',(-0.0866025403784438,-0.4,-0.15));
#22879=CARTESIAN_POINT('',(-0.173205080756888,-0.64,-2.77555756156289E-17));
#22880=CARTESIAN_POINT('',(-0.173205080756888,-0.4,-2.12115047744981E-17));
#22881=CARTESIAN_POINT('',(-0.0866025403784438,-0.64,-0.15));
#22882=CARTESIAN_POINT('Origin',(-0.0866025403784439,-0.4,0.15));
#22883=CARTESIAN_POINT('',(-0.0866025403784439,-0.4,0.15));
#22884=CARTESIAN_POINT('',(-0.173205080756888,-0.4,-2.12115047744981E-17));
#22885=CARTESIAN_POINT('',(-0.0866025403784439,-0.64,0.15));
#22886=CARTESIAN_POINT('',(-0.0866025403784439,-0.4,0.15));
#22887=CARTESIAN_POINT('',(-0.173205080756888,-0.64,-2.12115047744981E-17));
#22888=CARTESIAN_POINT('Origin',(0.0866025403784439,-0.4,0.15));
#22889=CARTESIAN_POINT('',(0.0866025403784439,-0.4,0.15));
#22890=CARTESIAN_POINT('',(-0.0866025403784439,-0.4,0.15));
#22891=CARTESIAN_POINT('',(0.0866025403784439,-0.64,0.15));
#22892=CARTESIAN_POINT('',(0.0866025403784439,-0.4,0.15));
#22893=CARTESIAN_POINT('',(-0.0866025403784439,-0.64,0.15));
#22894=CARTESIAN_POINT('Origin',(0.173205080756888,-0.4,0.));
#22895=CARTESIAN_POINT('',(0.0866025403784439,-0.4,0.15));
#22896=CARTESIAN_POINT('',(0.0866025403784439,-0.64,0.15));
#22897=CARTESIAN_POINT('Origin',(0.,-0.4,-2.77555756156289E-17));
#22898=CARTESIAN_POINT('Origin',(0.,-0.64,-2.77555756156289E-17));
#22899=CARTESIAN_POINT('',(0.,0.,0.));
#22900=CARTESIAN_POINT('',(0.,0.,0.));
#22901=CARTESIAN_POINT('',(0.,0.,0.));
#22902=CARTESIAN_POINT('',(0.,0.,0.));
#22903=CARTESIAN_POINT('',(0.,0.,0.));
#22904=CARTESIAN_POINT('',(0.,0.,0.));
#22905=CARTESIAN_POINT('',(0.,0.,0.));
#22906=CARTESIAN_POINT('',(0.,0.,0.));
#22907=CARTESIAN_POINT('',(0.,0.,0.));
#22908=CARTESIAN_POINT('',(0.,0.,0.));
#22909=CARTESIAN_POINT('',(0.,0.,0.));
#22910=CARTESIAN_POINT('',(0.,0.,0.));
#22911=CARTESIAN_POINT('',(0.,0.,0.));
#22912=CARTESIAN_POINT('',(0.,0.,0.));
#22913=CARTESIAN_POINT('',(0.,0.,0.));
#22914=CARTESIAN_POINT('',(0.,0.,0.));
#22915=CARTESIAN_POINT('',(0.,0.,0.));
#22916=CARTESIAN_POINT('',(0.,0.,0.));
#22917=CARTESIAN_POINT('',(0.,0.,0.));
#22918=CARTESIAN_POINT('',(0.,0.,0.));
#22919=CARTESIAN_POINT('',(0.,0.,0.));
#22920=CARTESIAN_POINT('',(0.,0.,0.));
#22921=CARTESIAN_POINT('',(0.,0.,0.));
#22922=CARTESIAN_POINT('',(0.,0.,0.));
#22923=CARTESIAN_POINT('',(0.,0.,0.));
#22924=CARTESIAN_POINT('',(0.,0.,0.));
#22925=CARTESIAN_POINT('',(0.,0.,0.));
#22926=CARTESIAN_POINT('',(0.,0.,0.));
#22927=CARTESIAN_POINT('',(0.,0.,0.));
#22928=CARTESIAN_POINT('',(-3.2,5.2,1.8));
#22929=CARTESIAN_POINT('',(-3.2,7.8,1.8));
#22930=CARTESIAN_POINT('',(3.2,5.2,1.8));
#22931=CARTESIAN_POINT('',(3.2,7.8,1.8));
#22932=CARTESIAN_POINT('',(14.8,5.2,1.8));
#22933=CARTESIAN_POINT('',(14.8,7.8,1.8));
#22934=CARTESIAN_POINT('',(21.2,5.2,1.8));
#22935=CARTESIAN_POINT('',(21.2,7.8,1.8));
#22936=CARTESIAN_POINT('',(1.15,4.1,15.));
#22937=CARTESIAN_POINT('',(-0.575,4.1,15.9959292143521));
#22938=CARTESIAN_POINT('',(-0.575000000000001,4.1,14.0040707856479));
#22939=CARTESIAN_POINT('',(0.,-1.2,15.));
#22940=CARTESIAN_POINT('',(19.15,4.1,15.));
#22941=CARTESIAN_POINT('',(17.425,4.1,15.9959292143521));
#22942=CARTESIAN_POINT('',(17.425,4.1,14.0040707856479));
#22943=CARTESIAN_POINT('',(18.,-1.2,15.));
#22944=CARTESIAN_POINT('',(-9.5,-4.5,8.));
#22945=CARTESIAN_POINT('',(-9.5,-8.2,1.8));
#22946=CARTESIAN_POINT('',(-9.5,-0.8,1.8));
#22947=CARTESIAN_POINT('',(0.5,-4.5,8.));
#22948=CARTESIAN_POINT('',(0.5,-8.2,1.8));
#22949=CARTESIAN_POINT('',(0.5,-0.8,1.8));
#22950=CARTESIAN_POINT('',(0.,0.,0.));
#22951=CARTESIAN_POINT('',(0.,0.,0.));
#22952=CARTESIAN_POINT('',(0.,0.,0.));
#22953=CARTESIAN_POINT('',(0.,0.,0.));
#22954=CARTESIAN_POINT('',(0.,0.,0.));
#22955=CARTESIAN_POINT('',(0.,0.,0.));
#22956=CARTESIAN_POINT('',(0.,0.,0.));
#22957=CARTESIAN_POINT('',(0.,0.,0.));
#22958=CARTESIAN_POINT('',(0.,0.,0.));
#22959=CARTESIAN_POINT('',(0.,0.,0.));
#22960=CARTESIAN_POINT('',(0.,0.,0.));
#22961=CARTESIAN_POINT('',(0.,0.,0.));
#22962=CARTESIAN_POINT('',(10.5469262078591,2.1,18.4202014332567));
#22963=CARTESIAN_POINT('',(8.82192620785908,2.1,19.4161306476088));
#22964=CARTESIAN_POINT('',(8.82192620785908,2.1,17.4242722189046));
#22965=CARTESIAN_POINT('',(9.39692620785909,-5.7,18.4202014332567));
#22966=CARTESIAN_POINT('',(25.3520784790221,2.1,28.6577532024872));
#22967=CARTESIAN_POINT('',(23.6270784790221,2.1,29.6536824168393));
#22968=CARTESIAN_POINT('',(23.6270784790221,2.1,27.6618239881351));
#22969=CARTESIAN_POINT('',(24.2020784790221,-1.2,28.6577532024872));
#22970=CARTESIAN_POINT('',(0.,0.,0.));
#22971=CARTESIAN_POINT('',(0.,0.,0.));
#22972=CARTESIAN_POINT('Origin',(-5.8,-4.5,8.));
#22973=CARTESIAN_POINT('',(-5.7,-4.5,8.5));
#22974=CARTESIAN_POINT('Origin',(-5.7,-4.5,8.));
#22975=CARTESIAN_POINT('',(-2.3,-4.5,8.5));
#22976=CARTESIAN_POINT('',(-5.8,-4.5,8.5));
#22977=CARTESIAN_POINT('Origin',(-2.3,-4.5,8.));
#22978=CARTESIAN_POINT('Origin',(-5.8,-7.,8.));
#22979=CARTESIAN_POINT('',(-5.7,-7.,9.05));
#22980=CARTESIAN_POINT('Origin',(-5.7,-7.,8.));
#22981=CARTESIAN_POINT('',(-2.3,-7.,9.05));
#22982=CARTESIAN_POINT('',(-5.8,-7.,9.05));
#22983=CARTESIAN_POINT('Origin',(-2.3,-7.,8.));
#22984=CARTESIAN_POINT('Origin',(-5.8,-2.,8.));
#22985=CARTESIAN_POINT('',(-5.7,-2.,9.05));
#22986=CARTESIAN_POINT('Origin',(-5.7,-2.,8.));
#22987=CARTESIAN_POINT('',(-2.3,-2.,9.05));
#22988=CARTESIAN_POINT('',(-5.8,-2.,9.05));
#22989=CARTESIAN_POINT('Origin',(-2.3,-2.,8.));
#22990=CARTESIAN_POINT('Origin',(-2.3,-0.8,6.3));
#22991=CARTESIAN_POINT('',(-2.3,-0.8,6.3));
#22992=CARTESIAN_POINT('',(-5.7,-0.8,6.3));
#22993=CARTESIAN_POINT('',(-2.3,-0.8,6.3));
#22994=CARTESIAN_POINT('',(-5.7,-0.8,9.7));
#22995=CARTESIAN_POINT('',(-5.7,-0.8,6.3));
#22996=CARTESIAN_POINT('',(-2.3,-0.8,9.7));
#22997=CARTESIAN_POINT('',(-2.3,-0.8,9.7));
#22998=CARTESIAN_POINT('',(-2.3,-0.8,6.3));
#22999=CARTESIAN_POINT('Origin',(-2.3,-8.2,6.3));
#23000=CARTESIAN_POINT('',(-2.3,-8.2,6.3));
#23001=CARTESIAN_POINT('',(-2.3,-8.2,6.3));
#23002=CARTESIAN_POINT('',(-2.3,-8.2,9.7));
#23003=CARTESIAN_POINT('',(-2.3,-8.2,9.7));
#23004=CARTESIAN_POINT('',(-2.3,-8.2,6.3));
#23005=CARTESIAN_POINT('Origin',(-5.7,-8.2,6.3));
#23006=CARTESIAN_POINT('',(-5.7,-8.2,6.3));
#23007=CARTESIAN_POINT('',(-5.7,-8.2,6.3));
#23008=CARTESIAN_POINT('',(-5.7,-8.2,9.7));
#23009=CARTESIAN_POINT('',(-5.7,-8.2,9.7));
#23010=CARTESIAN_POINT('',(-5.7,-8.2,6.3));
#23011=CARTESIAN_POINT('Origin',(-5.7,-0.8,6.3));
#23012=CARTESIAN_POINT('',(-5.7,-0.8,6.3));
#23013=CARTESIAN_POINT('',(-5.7,-0.8,9.7));
#23014=CARTESIAN_POINT('Origin',(-4.,-4.5,9.7));
#23015=CARTESIAN_POINT('Origin',(-4.,-4.5,6.3));
#23016=CARTESIAN_POINT('',(0.,0.,0.));
#23017=CARTESIAN_POINT('Origin',(-6.,-4.5,8.));
#23018=CARTESIAN_POINT('',(-5.9,-4.5,8.65));
#23019=CARTESIAN_POINT('Origin',(-5.9,-4.5,8.));
#23020=CARTESIAN_POINT('',(-5.7,-4.5,8.65));
#23021=CARTESIAN_POINT('',(-6.,-4.5,8.65));
#23022=CARTESIAN_POINT('Origin',(-5.7,-4.5,8.));
#23023=CARTESIAN_POINT('Origin',(-6.,-7.,8.));
#23024=CARTESIAN_POINT('',(-5.9,-7.,8.8));
#23025=CARTESIAN_POINT('Origin',(-5.9,-7.,8.));
#23026=CARTESIAN_POINT('',(-5.7,-7.,8.8));
#23027=CARTESIAN_POINT('',(-6.,-7.,8.8));
#23028=CARTESIAN_POINT('Origin',(-5.7,-7.,8.));
#23029=CARTESIAN_POINT('Origin',(-6.,-2.,8.));
#23030=CARTESIAN_POINT('',(-5.9,-2.,8.8));
#23031=CARTESIAN_POINT('Origin',(-5.9,-2.,8.));
#23032=CARTESIAN_POINT('',(-5.7,-2.,8.8));
#23033=CARTESIAN_POINT('',(-6.,-2.,8.8));
#23034=CARTESIAN_POINT('Origin',(-5.7,-2.,8.));
#23035=CARTESIAN_POINT('Origin',(-5.9,-0.8,9.7));
#23036=CARTESIAN_POINT('',(-5.9,-0.8,9.7));
#23037=CARTESIAN_POINT('',(-5.9,-8.2,9.7));
#23038=CARTESIAN_POINT('',(-5.9,-0.8,9.7));
#23039=CARTESIAN_POINT('',(-5.7,-8.2,9.7));
#23040=CARTESIAN_POINT('',(-5.9,-8.2,9.7));
#23041=CARTESIAN_POINT('',(-5.7,-0.8,9.7));
#23042=CARTESIAN_POINT('',(-5.7,-0.8,9.7));
#23043=CARTESIAN_POINT('',(-5.9,-0.8,9.7));
#23044=CARTESIAN_POINT('Origin',(-5.9,-0.8,6.3));
#23045=CARTESIAN_POINT('',(-5.9,-0.8,6.3));
#23046=CARTESIAN_POINT('',(-5.9,-0.8,6.3));
#23047=CARTESIAN_POINT('',(-5.7,-0.8,6.3));
#23048=CARTESIAN_POINT('',(-5.7,-0.8,6.3));
#23049=CARTESIAN_POINT('',(-5.9,-0.8,6.3));
#23050=CARTESIAN_POINT('Origin',(-5.9,-8.2,6.3));
#23051=CARTESIAN_POINT('',(-5.9,-8.2,6.3));
#23052=CARTESIAN_POINT('',(-5.9,-8.2,6.3));
#23053=CARTESIAN_POINT('',(-5.7,-8.2,6.3));
#23054=CARTESIAN_POINT('',(-5.7,-8.2,6.3));
#23055=CARTESIAN_POINT('',(-5.9,-8.2,6.3));
#23056=CARTESIAN_POINT('Origin',(-5.9,-8.2,9.7));
#23057=CARTESIAN_POINT('',(-5.9,-8.2,9.7));
#23058=CARTESIAN_POINT('',(-5.7,-8.2,9.7));
#23059=CARTESIAN_POINT('Origin',(-5.7,-4.5,8.));
#23060=CARTESIAN_POINT('Origin',(-5.9,-4.5,8.));
#23061=CARTESIAN_POINT('',(0.,0.,0.));
#23062=CARTESIAN_POINT('Origin',(-2.4,-4.5,8.));
#23063=CARTESIAN_POINT('',(-2.3,-4.5,8.65));
#23064=CARTESIAN_POINT('Origin',(-2.3,-4.5,8.));
#23065=CARTESIAN_POINT('',(-2.1,-4.5,8.65));
#23066=CARTESIAN_POINT('',(-2.4,-4.5,8.65));
#23067=CARTESIAN_POINT('Origin',(-2.1,-4.5,8.));
#23068=CARTESIAN_POINT('Origin',(-2.4,-7.,8.));
#23069=CARTESIAN_POINT('',(-2.3,-7.,8.8));
#23070=CARTESIAN_POINT('Origin',(-2.3,-7.,8.));
#23071=CARTESIAN_POINT('',(-2.1,-7.,8.8));
#23072=CARTESIAN_POINT('',(-2.4,-7.,8.8));
#23073=CARTESIAN_POINT('Origin',(-2.1,-7.,8.));
#23074=CARTESIAN_POINT('Origin',(-2.4,-2.,8.));
#23075=CARTESIAN_POINT('',(-2.3,-2.,8.8));
#23076=CARTESIAN_POINT('Origin',(-2.3,-2.,8.));
#23077=CARTESIAN_POINT('',(-2.1,-2.,8.8));
#23078=CARTESIAN_POINT('',(-2.4,-2.,8.8));
#23079=CARTESIAN_POINT('Origin',(-2.1,-2.,8.));
#23080=CARTESIAN_POINT('Origin',(-2.3,-0.8,9.7));
#23081=CARTESIAN_POINT('',(-2.3,-0.8,9.7));
#23082=CARTESIAN_POINT('',(-2.3,-8.2,9.7));
#23083=CARTESIAN_POINT('',(-2.3,-0.8,9.7));
#23084=CARTESIAN_POINT('',(-2.1,-8.2,9.7));
#23085=CARTESIAN_POINT('',(-2.3,-8.2,9.7));
#23086=CARTESIAN_POINT('',(-2.1,-0.8,9.7));
#23087=CARTESIAN_POINT('',(-2.1,-0.8,9.7));
#23088=CARTESIAN_POINT('',(-2.3,-0.8,9.7));
#23089=CARTESIAN_POINT('Origin',(-2.3,-0.8,6.3));
#23090=CARTESIAN_POINT('',(-2.3,-0.8,6.3));
#23091=CARTESIAN_POINT('',(-2.3,-0.8,6.3));
#23092=CARTESIAN_POINT('',(-2.1,-0.8,6.3));
#23093=CARTESIAN_POINT('',(-2.1,-0.8,6.3));
#23094=CARTESIAN_POINT('',(-2.3,-0.8,6.3));
#23095=CARTESIAN_POINT('Origin',(-2.3,-8.2,6.3));
#23096=CARTESIAN_POINT('',(-2.3,-8.2,6.3));
#23097=CARTESIAN_POINT('',(-2.3,-8.2,6.3));
#23098=CARTESIAN_POINT('',(-2.1,-8.2,6.3));
#23099=CARTESIAN_POINT('',(-2.1,-8.2,6.3));
#23100=CARTESIAN_POINT('',(-2.3,-8.2,6.3));
#23101=CARTESIAN_POINT('Origin',(-2.3,-8.2,9.7));
#23102=CARTESIAN_POINT('',(-2.3,-8.2,9.7));
#23103=CARTESIAN_POINT('',(-2.1,-8.2,9.7));
#23104=CARTESIAN_POINT('Origin',(-2.1,-4.5,8.));
#23105=CARTESIAN_POINT('Origin',(-2.3,-4.5,8.));
#23106=CARTESIAN_POINT('',(0.,0.,0.));
#23107=CARTESIAN_POINT('Origin',(-4.,-4.,11.));
#23108=CARTESIAN_POINT('',(-4.305,-3.9,11.));
#23109=CARTESIAN_POINT('Origin',(-4.,-3.9,11.));
#23110=CARTESIAN_POINT('',(-4.305,-3.,11.));
#23111=CARTESIAN_POINT('',(-4.305,-4.,11.));
#23112=CARTESIAN_POINT('Origin',(-4.,-3.,11.));
#23113=CARTESIAN_POINT('Origin',(-3.3,-3.,9.7));
#23114=CARTESIAN_POINT('',(-3.3,-3.,9.7));
#23115=CARTESIAN_POINT('',(-4.7,-3.,9.7));
#23116=CARTESIAN_POINT('',(-3.3,-3.,9.7));
#23117=CARTESIAN_POINT('',(-4.7,-3.,12.));
#23118=CARTESIAN_POINT('',(-4.7,-3.,9.7));
#23119=CARTESIAN_POINT('',(-3.3,-3.,12.));
#23120=CARTESIAN_POINT('',(-3.3,-3.,12.));
#23121=CARTESIAN_POINT('',(-3.3,-3.,9.7));
#23122=CARTESIAN_POINT('Origin',(-3.3,-3.9,9.7));
#23123=CARTESIAN_POINT('',(-3.3,-3.9,9.7));
#23124=CARTESIAN_POINT('',(-3.3,-3.9,9.7));
#23125=CARTESIAN_POINT('',(-3.3,-3.9,12.));
#23126=CARTESIAN_POINT('',(-3.3,-3.9,12.));
#23127=CARTESIAN_POINT('',(-3.3,-3.9,9.7));
#23128=CARTESIAN_POINT('Origin',(-4.7,-3.9,9.7));
#23129=CARTESIAN_POINT('',(-4.7,-3.9,9.7));
#23130=CARTESIAN_POINT('',(-4.7,-3.9,9.7));
#23131=CARTESIAN_POINT('',(-4.7,-3.9,12.));
#23132=CARTESIAN_POINT('',(-4.7,-3.9,12.));
#23133=CARTESIAN_POINT('',(-4.7,-3.9,9.7));
#23134=CARTESIAN_POINT('Origin',(-4.7,-3.,9.7));
#23135=CARTESIAN_POINT('',(-4.7,-3.,9.7));
#23136=CARTESIAN_POINT('',(-4.7,-3.,12.));
#23137=CARTESIAN_POINT('Origin',(-4.,-3.45,12.));
#23138=CARTESIAN_POINT('Origin',(-4.,-3.45,9.7));
#23139=CARTESIAN_POINT('',(0.,0.,0.));
#23140=CARTESIAN_POINT('Origin',(-4.,-4.1,11.));
#23141=CARTESIAN_POINT('',(-4.165,-4.1,11.));
#23142=CARTESIAN_POINT('Origin',(-4.,-4.1,11.));
#23143=CARTESIAN_POINT('',(-4.165,-3.,11.));
#23144=CARTESIAN_POINT('',(-4.165,-4.1,11.));
#23145=CARTESIAN_POINT('Origin',(-4.,-3.,11.));
#23146=CARTESIAN_POINT('Origin',(-4.,-4.1,11.));
#23147=CARTESIAN_POINT('Origin',(-4.,-5.2,11.));
#23148=CARTESIAN_POINT('',(-4.5,-5.2,11.));
#23149=CARTESIAN_POINT('Origin',(-4.,-5.2,11.));
#23150=CARTESIAN_POINT('',(-4.3,-5.2,11.));
#23151=CARTESIAN_POINT('Origin',(-4.,-5.2,11.));
#23152=CARTESIAN_POINT('Origin',(-4.,-5.4,11.));
#23153=CARTESIAN_POINT('',(-4.5,-5.4,11.));
#23154=CARTESIAN_POINT('',(-4.5,-5.4,11.));
#23155=CARTESIAN_POINT('Origin',(-4.,-5.4,11.));
#23156=CARTESIAN_POINT('Origin',(-4.,-5.4,11.));
#23157=CARTESIAN_POINT('Origin',(-4.,-5.2,11.));
#23158=CARTESIAN_POINT('',(-4.3,-3.,11.));
#23159=CARTESIAN_POINT('Origin',(-4.,-3.,11.));
#23160=CARTESIAN_POINT('',(-4.3,-5.2,11.));
#23161=CARTESIAN_POINT('Origin',(-4.,-3.,11.));
#23162=CARTESIAN_POINT('',(0.,0.,0.));
#23163=CARTESIAN_POINT('Origin',(-4.,-3.,11.));
#23164=CARTESIAN_POINT('',(-4.225,-2.8,11.));
#23165=CARTESIAN_POINT('Origin',(-4.,-2.8,11.));
#23166=CARTESIAN_POINT('',(-4.225,-3.,11.));
#23167=CARTESIAN_POINT('',(-4.225,-3.,11.));
#23168=CARTESIAN_POINT('Origin',(-4.,-3.,11.));
#23169=CARTESIAN_POINT('Origin',(-4.,-3.,11.));
#23170=CARTESIAN_POINT('',(-4.6,-2.8,11.));
#23171=CARTESIAN_POINT('Origin',(-4.,-2.8,11.));
#23172=CARTESIAN_POINT('',(-4.6,-3.,11.));
#23173=CARTESIAN_POINT('',(-4.6,-3.,11.));
#23174=CARTESIAN_POINT('Origin',(-4.,-3.,11.));
#23175=CARTESIAN_POINT('Origin',(-4.,-2.8,11.));
#23176=CARTESIAN_POINT('Origin',(-4.,-3.,11.));
#23177=CARTESIAN_POINT('',(0.,0.,0.));
#23178=CARTESIAN_POINT('Origin',(-4.,-5.2,11.));
#23179=CARTESIAN_POINT('',(-4.305,-5.,11.));
#23180=CARTESIAN_POINT('Origin',(-4.,-5.,11.));
#23181=CARTESIAN_POINT('',(-4.305,-5.2,11.));
#23182=CARTESIAN_POINT('',(-4.305,-5.2,11.));
#23183=CARTESIAN_POINT('Origin',(-4.,-5.2,11.));
#23184=CARTESIAN_POINT('Origin',(-4.,-5.2,11.));
#23185=CARTESIAN_POINT('',(-4.45,-5.,11.));
#23186=CARTESIAN_POINT('Origin',(-4.,-5.,11.));
#23187=CARTESIAN_POINT('',(-4.45,-5.2,11.));
#23188=CARTESIAN_POINT('',(-4.45,-5.2,11.));
#23189=CARTESIAN_POINT('Origin',(-4.,-5.2,11.));
#23190=CARTESIAN_POINT('Origin',(-4.,-5.,11.));
#23191=CARTESIAN_POINT('Origin',(-4.,-5.2,11.));
#23192=CARTESIAN_POINT('',(0.,0.,0.));
#23193=CARTESIAN_POINT('',(0.,0.,0.));
#23194=CARTESIAN_POINT('Origin',(0.75,1.2,0.));
#23195=CARTESIAN_POINT('',(0.885663593019381,1.2,-0.16));
#23196=CARTESIAN_POINT('',(0.885663593019381,1.2,0.16));
#23197=CARTESIAN_POINT('Origin',(0.,1.2,0.));
#23198=CARTESIAN_POINT('',(0.93,1.2,-0.16));
#23199=CARTESIAN_POINT('',(0.93,1.2,-0.16));
#23200=CARTESIAN_POINT('',(0.93,1.2,0.16));
#23201=CARTESIAN_POINT('',(0.93,1.2,0.16));
#23202=CARTESIAN_POINT('',(0.57,1.2,0.16));
#23203=CARTESIAN_POINT('Origin',(0.57,0.,0.16));
#23204=CARTESIAN_POINT('',(0.885663593019381,-1.2,0.16));
#23205=CARTESIAN_POINT('',(0.885663593019381,0.,0.16));
#23206=CARTESIAN_POINT('',(0.93,-1.2,0.16));
#23207=CARTESIAN_POINT('',(0.93,0.,0.16));
#23208=CARTESIAN_POINT('',(0.57,-1.2,0.16));
#23209=CARTESIAN_POINT('Origin',(0.75,-1.2,0.));
#23210=CARTESIAN_POINT('',(0.885663593019381,-1.2,-0.16));
#23211=CARTESIAN_POINT('Origin',(0.,-1.2,0.));
#23212=CARTESIAN_POINT('',(0.93,-1.2,-0.16));
#23213=CARTESIAN_POINT('',(0.93,-1.2,0.16));
#23214=CARTESIAN_POINT('',(0.93,-1.2,-0.16));
#23215=CARTESIAN_POINT('Origin',(0.93,0.,-0.16));
#23216=CARTESIAN_POINT('',(0.885663593019381,0.,-0.16));
#23217=CARTESIAN_POINT('',(0.93,0.,-0.16));
#23218=CARTESIAN_POINT('Origin',(0.93,0.,0.16));
#23219=CARTESIAN_POINT('Origin',(1.05,1.5,0.));
#23220=CARTESIAN_POINT('',(-1.05,1.5,-1.28587913910472E-16));
#23221=CARTESIAN_POINT('Origin',(0.,1.5,0.));
#23222=CARTESIAN_POINT('',(-0.9,1.5,-1.10218211923262E-16));
#23223=CARTESIAN_POINT('Origin',(0.,1.5,0.));
#23224=CARTESIAN_POINT('Origin',(0.,1.315,0.));
#23225=CARTESIAN_POINT('',(-1.05,1.13,-1.28587913910472E-16));
#23226=CARTESIAN_POINT('Origin',(0.,1.13,0.));
#23227=CARTESIAN_POINT('',(-1.05,1.315,-1.28587913910472E-16));
#23228=CARTESIAN_POINT('Origin',(1.,1.13,0.));
#23229=CARTESIAN_POINT('',(-1.,1.13,-1.22464679914735E-16));
#23230=CARTESIAN_POINT('Origin',(0.,1.13,0.));
#23231=CARTESIAN_POINT('Origin',(0.,1.065,0.));
#23232=CARTESIAN_POINT('',(-1.,1.,-1.22464679914735E-16));
#23233=CARTESIAN_POINT('Origin',(0.,1.,0.));
#23234=CARTESIAN_POINT('',(-1.,1.065,-1.22464679914735E-16));
#23235=CARTESIAN_POINT('Origin',(1.05,1.,0.));
#23236=CARTESIAN_POINT('',(-1.05,1.,-1.28587913910472E-16));
#23237=CARTESIAN_POINT('Origin',(0.,1.,0.));
#23238=CARTESIAN_POINT('Origin',(0.,0.,0.));
#23239=CARTESIAN_POINT('',(-1.05,-1.,-1.28587913910472E-16));
#23240=CARTESIAN_POINT('Origin',(0.,-1.,0.));
#23241=CARTESIAN_POINT('',(-1.05,0.,-1.28587913910472E-16));
#23242=CARTESIAN_POINT('Origin',(1.,-1.,0.));
#23243=CARTESIAN_POINT('',(-1.,-1.,-1.22464679914735E-16));
#23244=CARTESIAN_POINT('Origin',(0.,-1.,0.));
#23245=CARTESIAN_POINT('Origin',(0.,-1.065,0.));
#23246=CARTESIAN_POINT('',(-1.,-1.13,-1.22464679914735E-16));
#23247=CARTESIAN_POINT('Origin',(0.,-1.13,0.));
#23248=CARTESIAN_POINT('',(-1.,-1.065,-1.22464679914735E-16));
#23249=CARTESIAN_POINT('Origin',(1.05,-1.13,0.));
#23250=CARTESIAN_POINT('',(-1.05,-1.13,-1.28587913910472E-16));
#23251=CARTESIAN_POINT('Origin',(0.,-1.13,0.));
#23252=CARTESIAN_POINT('Origin',(0.,-1.315,0.));
#23253=CARTESIAN_POINT('',(-1.05,-1.5,-1.28587913910472E-16));
#23254=CARTESIAN_POINT('Origin',(0.,-1.5,0.));
#23255=CARTESIAN_POINT('',(-1.05,-1.315,-1.28587913910472E-16));
#23256=CARTESIAN_POINT('Origin',(0.9,-1.5,0.));
#23257=CARTESIAN_POINT('',(-0.9,-1.5,-1.10218211923262E-16));
#23258=CARTESIAN_POINT('Origin',(0.,-1.5,0.));
#23259=CARTESIAN_POINT('Origin',(0.,0.,0.));
#23260=CARTESIAN_POINT('',(-0.9,0.,-1.10218211923262E-16));
#23261=CARTESIAN_POINT('',(0.,0.,0.));
#23262=CARTESIAN_POINT('Origin',(0.75,1.2,0.));
#23263=CARTESIAN_POINT('',(0.880582193778639,1.2,0.16));
#23264=CARTESIAN_POINT('',(0.880582193778639,1.2,-0.16));
#23265=CARTESIAN_POINT('Origin',(0.,1.2,0.));
#23266=CARTESIAN_POINT('',(0.583459510163302,1.2,0.16));
#23267=CARTESIAN_POINT('',(0.57,1.2,0.16));
#23268=CARTESIAN_POINT('',(0.583459510163302,1.2,-0.16));
#23269=CARTESIAN_POINT('Origin',(0.,1.2,0.));
#23270=CARTESIAN_POINT('',(0.93,1.2,-0.16));
#23271=CARTESIAN_POINT('Origin',(0.93,0.,-0.16));
#23272=CARTESIAN_POINT('',(0.880582193778639,-1.2,-0.16));
#23273=CARTESIAN_POINT('',(0.880582193778639,0.,-0.16));
#23274=CARTESIAN_POINT('',(0.583459510163302,-1.2,-0.16));
#23275=CARTESIAN_POINT('',(0.583459510163302,0.,-0.16));
#23276=CARTESIAN_POINT('',(0.93,-1.2,-0.16));
#23277=CARTESIAN_POINT('Origin',(0.75,-1.2,0.));
#23278=CARTESIAN_POINT('',(0.880582193778639,-1.2,0.16));
#23279=CARTESIAN_POINT('Origin',(0.,-1.2,0.));
#23280=CARTESIAN_POINT('',(0.583459510163302,-1.2,0.16));
#23281=CARTESIAN_POINT('Origin',(0.,-1.2,0.));
#23282=CARTESIAN_POINT('',(0.57,-1.2,0.16));
#23283=CARTESIAN_POINT('Origin',(0.57,0.,0.16));
#23284=CARTESIAN_POINT('',(0.880582193778639,0.,0.16));
#23285=CARTESIAN_POINT('',(0.583459510163302,0.,0.16));
#23286=CARTESIAN_POINT('Origin',(0.895,1.35,0.));
#23287=CARTESIAN_POINT('',(-0.895,1.35,-1.09605888523688E-16));
#23288=CARTESIAN_POINT('Origin',(0.,1.35,0.));
#23289=CARTESIAN_POINT('',(-0.605,1.35,-7.40911313484149E-17));
#23290=CARTESIAN_POINT('Origin',(0.,1.35,0.));
#23291=CARTESIAN_POINT('Origin',(0.,0.,0.));
#23292=CARTESIAN_POINT('',(-0.895,-1.35,-1.09605888523688E-16));
#23293=CARTESIAN_POINT('Origin',(0.,-1.35,0.));
#23294=CARTESIAN_POINT('',(-0.895,0.,-1.09605888523688E-16));
#23295=CARTESIAN_POINT('Origin',(0.605,-1.35,0.));
#23296=CARTESIAN_POINT('',(-0.605,-1.35,-7.40911313484149E-17));
#23297=CARTESIAN_POINT('Origin',(0.,-1.35,0.));
#23298=CARTESIAN_POINT('Origin',(0.,0.,0.));
#23299=CARTESIAN_POINT('',(-0.605,0.,-7.40911313484149E-17));
#23300=CARTESIAN_POINT('',(0.,0.,0.));
#23301=CARTESIAN_POINT('',(0.,0.,0.));
#23302=CARTESIAN_POINT('',(0.,0.,0.));
#23303=CARTESIAN_POINT('Origin',(0.0866025403784439,-0.4,-0.15));
#23304=CARTESIAN_POINT('',(0.173205080756888,-0.4,0.));
#23305=CARTESIAN_POINT('',(0.0866025403784439,-0.4,-0.15));
#23306=CARTESIAN_POINT('',(0.173205080756888,-0.4,0.));
#23307=CARTESIAN_POINT('',(0.0866025403784439,-0.64,-0.15));
#23308=CARTESIAN_POINT('',(0.0866025403784439,-0.4,-0.15));
#23309=CARTESIAN_POINT('',(0.173205080756888,-0.64,0.));
#23310=CARTESIAN_POINT('',(0.173205080756888,-0.64,0.));
#23311=CARTESIAN_POINT('',(0.173205080756888,-0.4,0.));
#23312=CARTESIAN_POINT('Origin',(-0.0866025403784438,-0.4,-0.15));
#23313=CARTESIAN_POINT('',(-0.0866025403784438,-0.4,-0.15));
#23314=CARTESIAN_POINT('',(0.0866025403784439,-0.4,-0.15));
#23315=CARTESIAN_POINT('',(-0.0866025403784438,-0.64,-0.15));
#23316=CARTESIAN_POINT('',(-0.0866025403784438,-0.4,-0.15));
#23317=CARTESIAN_POINT('',(0.0866025403784439,-0.64,-0.15));
#23318=CARTESIAN_POINT('Origin',(-0.173205080756888,-0.4,-2.77555756156289E-17));
#23319=CARTESIAN_POINT('',(-0.173205080756888,-0.4,-2.12115047744981E-17));
#23320=CARTESIAN_POINT('',(-0.0866025403784438,-0.4,-0.15));
#23321=CARTESIAN_POINT('',(-0.173205080756888,-0.64,-2.77555756156289E-17));
#23322=CARTESIAN_POINT('',(-0.173205080756888,-0.4,-2.12115047744981E-17));
#23323=CARTESIAN_POINT('',(-0.0866025403784438,-0.64,-0.15));
#23324=CARTESIAN_POINT('Origin',(-0.0866025403784439,-0.4,0.15));
#23325=CARTESIAN_POINT('',(-0.0866025403784439,-0.4,0.15));
#23326=CARTESIAN_POINT('',(-0.173205080756888,-0.4,-2.12115047744981E-17));
#23327=CARTESIAN_POINT('',(-0.0866025403784439,-0.64,0.15));
#23328=CARTESIAN_POINT('',(-0.0866025403784439,-0.4,0.15));
#23329=CARTESIAN_POINT('',(-0.173205080756888,-0.64,-2.12115047744981E-17));
#23330=CARTESIAN_POINT('Origin',(0.0866025403784439,-0.4,0.15));
#23331=CARTESIAN_POINT('',(0.0866025403784439,-0.4,0.15));
#23332=CARTESIAN_POINT('',(-0.0866025403784439,-0.4,0.15));
#23333=CARTESIAN_POINT('',(0.0866025403784439,-0.64,0.15));
#23334=CARTESIAN_POINT('',(0.0866025403784439,-0.4,0.15));
#23335=CARTESIAN_POINT('',(-0.0866025403784439,-0.64,0.15));
#23336=CARTESIAN_POINT('Origin',(0.173205080756888,-0.4,0.));
#23337=CARTESIAN_POINT('',(0.0866025403784439,-0.4,0.15));
#23338=CARTESIAN_POINT('',(0.0866025403784439,-0.64,0.15));
#23339=CARTESIAN_POINT('Origin',(0.,-0.4,-2.77555756156289E-17));
#23340=CARTESIAN_POINT('Origin',(0.,-0.64,-2.77555756156289E-17));
#23341=CARTESIAN_POINT('Origin',(0.,-1.,0.));
#23342=CARTESIAN_POINT('',(-0.1954,-1.,2.39295984553393E-17));
#23343=CARTESIAN_POINT('Origin',(0.,-1.,0.));
#23344=CARTESIAN_POINT('Origin',(0.3,0.4,0.));
#23345=CARTESIAN_POINT('',(-0.3,0.4,-3.67394039744206E-17));
#23346=CARTESIAN_POINT('Origin',(0.,0.4,0.));
#23347=CARTESIAN_POINT('Origin',(0.,0.375,0.));
#23348=CARTESIAN_POINT('',(-0.35,0.35,-4.28626379701573E-17));
#23349=CARTESIAN_POINT('Origin',(0.,0.35,0.));
#23350=CARTESIAN_POINT('',(-0.325,0.375,-3.9801020972289E-17));
#23351=CARTESIAN_POINT('Origin',(0.,0.19,0.));
#23352=CARTESIAN_POINT('',(-0.35,0.03,-4.28626379701574E-17));
#23353=CARTESIAN_POINT('Origin',(0.,0.03,0.));
#23354=CARTESIAN_POINT('',(-0.35,0.19,-4.28626379701574E-17));
#23355=CARTESIAN_POINT('Origin',(0.,0.0149999999999999,0.));
#23356=CARTESIAN_POINT('',(-0.32,-3.29597460435593E-17,-3.91886975727153E-17));
#23357=CARTESIAN_POINT('Origin',(0.,0.,0.));
#23358=CARTESIAN_POINT('',(-0.335,0.0149999999999999,-4.10256677714363E-17));
#23359=CARTESIAN_POINT('Origin',(0.22,0.,0.));
#23360=CARTESIAN_POINT('',(-0.22,-6.93889390390723E-18,-2.69422295812418E-17));
#23361=CARTESIAN_POINT('Origin',(0.,0.,0.));
#23362=CARTESIAN_POINT('Origin',(0.,-0.02,0.));
#23363=CARTESIAN_POINT('',(-0.1954,-0.0492,2.39295984553393E-17));
#23364=CARTESIAN_POINT('Origin',(0.,-0.0492,0.));
#23365=CARTESIAN_POINT('',(-0.21,-0.02,-2.57175827820944E-17));
#23366=CARTESIAN_POINT('Origin',(0.,-0.8,0.));
#23367=CARTESIAN_POINT('',(-0.1954,-0.8,-2.39295984553393E-17));
#23368=CARTESIAN_POINT('',(0.,0.,0.));
#23369=CARTESIAN_POINT('',(0.,0.,0.));
#23370=CARTESIAN_POINT('',(0.,0.,0.));
#23371=CARTESIAN_POINT('',(0.,0.,0.));
#23372=CARTESIAN_POINT('',(0.,0.,0.));
#23373=CARTESIAN_POINT('',(0.,0.,0.));
#23374=CARTESIAN_POINT('',(0.,0.,0.));
#23375=CARTESIAN_POINT('',(-4.,-7.,8.));
#23376=CARTESIAN_POINT('',(-4.,-2.,8.));
#23377=CARTESIAN_POINT('',(-4.,-2.8,11.));
#23378=CARTESIAN_POINT('',(0.,0.,0.));
#23379=CARTESIAN_POINT('',(0.,0.,0.));
#23380=CARTESIAN_POINT('Origin',(9.39692620785909,-5.1,18.4202014332567));
#23381=CARTESIAN_POINT('',(8.79192620785908,-5.,18.4202014332567));
#23382=CARTESIAN_POINT('Origin',(9.39692620785909,-5.,18.4202014332567));
#23383=CARTESIAN_POINT('',(8.79192620785908,-4.,18.4202014332567));
#23384=CARTESIAN_POINT('',(8.79192620785908,-5.1,18.4202014332567));
#23385=CARTESIAN_POINT('Origin',(9.39692620785909,-4.,18.4202014332567));
#23386=CARTESIAN_POINT('Origin',(9.39692620785909,-5.,18.4202014332567));
#23387=CARTESIAN_POINT('',(8.99381236827096,-4.,17.3967273337639));
#23388=CARTESIAN_POINT('',(8.99381236827096,-5.,17.3967273337639));
#23389=CARTESIAN_POINT('',(8.99381236827096,-5.,17.3967273337639));
#23390=CARTESIAN_POINT('',(8.31548704836563,-4.,18.6214210752256));
#23391=CARTESIAN_POINT('Origin',(9.39692620785909,-4.,18.4202014332567));
#23392=CARTESIAN_POINT('',(8.31548704836563,-5.,18.6214210752256));
#23393=CARTESIAN_POINT('',(8.31548704836563,-5.,18.6214210752256));
#23394=CARTESIAN_POINT('Origin',(9.39692620785909,-5.,18.4202014332567));
#23395=CARTESIAN_POINT('Origin',(2.69846310392954,-5.,14.7101007166283));
#23396=CARTESIAN_POINT('',(-4.00036134103228,-5.,11.7999999183954));
#23397=CARTESIAN_POINT('',(-4.33916265995267,-5.,11.6123468707308));
#23398=CARTESIAN_POINT('',(-3.32203602112695,-5.,10.5753061769338));
#23399=CARTESIAN_POINT('Origin',(-4.,-5.,11.));
#23400=CARTESIAN_POINT('',(9.73608886781175,-5.,17.8078545625259));
#23401=CARTESIAN_POINT('',(-4.305,-5.,11.));
#23402=CARTESIAN_POINT('Origin',(-4.,-5.,11.));
#23403=CARTESIAN_POINT('Origin',(-4.33916265995267,-5.,11.6123468707308));
#23404=CARTESIAN_POINT('',(-4.00036134103228,-4.,11.7999999183954));
#23405=CARTESIAN_POINT('',(-4.33916265995267,-4.,11.6123468707308));
#23406=CARTESIAN_POINT('',(-4.00036134103228,-5.,11.7999999183954));
#23407=CARTESIAN_POINT('Origin',(-4.,-5.1,11.));
#23408=CARTESIAN_POINT('',(-4.305,-4.,11.));
#23409=CARTESIAN_POINT('',(-4.305,-5.1,11.));
#23410=CARTESIAN_POINT('Origin',(-4.,-4.,11.));
#23411=CARTESIAN_POINT('Origin',(-4.,-5.,11.));
#23412=CARTESIAN_POINT('',(-3.32203602112695,-4.,10.5753061769338));
#23413=CARTESIAN_POINT('',(-3.32203602112695,-5.,10.5753061769338));
#23414=CARTESIAN_POINT('Origin',(-4.,-4.,11.));
#23415=CARTESIAN_POINT('Origin',(9.73608886781175,-5.,17.8078545625259));
#23416=CARTESIAN_POINT('',(9.73608886781175,-4.,17.8078545625259));
#23417=CARTESIAN_POINT('Origin',(2.69846310392954,-4.,14.7101007166283));
#23418=CARTESIAN_POINT('',(0.,0.,0.));
#23419=CARTESIAN_POINT('',(0.,0.,0.));
#23420=CARTESIAN_POINT('',(0.,0.,0.));
#23421=CARTESIAN_POINT('Origin',(-12.5,-4.5,8.));
#23422=CARTESIAN_POINT('',(2.,-4.5,8.6));
#23423=CARTESIAN_POINT('Origin',(2.,-4.5,8.));
#23424=CARTESIAN_POINT('',(-12.5,-4.5,8.6));
#23425=CARTESIAN_POINT('',(-12.5,-4.5,8.6));
#23426=CARTESIAN_POINT('Origin',(-12.5,-4.5,8.));
#23427=CARTESIAN_POINT('Origin',(2.,-4.5,8.));
#23428=CARTESIAN_POINT('Origin',(-12.5,-4.5,8.));
#23429=CARTESIAN_POINT('',(0.,0.,0.));
#23430=CARTESIAN_POINT('Origin',(-10.2,-4.5,8.));
#23431=CARTESIAN_POINT('',(-10.,-4.5,8.6));
#23432=CARTESIAN_POINT('Origin',(-10.,-4.5,8.));
#23433=CARTESIAN_POINT('',(-10.2,-4.5,8.6));
#23434=CARTESIAN_POINT('',(-10.2,-4.5,8.6));
#23435=CARTESIAN_POINT('Origin',(-10.2,-4.5,8.));
#23436=CARTESIAN_POINT('Origin',(-10.2,-4.5,8.));
#23437=CARTESIAN_POINT('',(-10.,-4.5,8.9));
#23438=CARTESIAN_POINT('Origin',(-10.,-4.5,8.));
#23439=CARTESIAN_POINT('',(-10.2,-4.5,8.9));
#23440=CARTESIAN_POINT('',(-10.2,-4.5,8.9));
#23441=CARTESIAN_POINT('Origin',(-10.2,-4.5,8.));
#23442=CARTESIAN_POINT('Origin',(-10.,-4.5,8.));
#23443=CARTESIAN_POINT('Origin',(-10.2,-4.5,8.));
#23444=CARTESIAN_POINT('',(0.,0.,0.));
#23445=CARTESIAN_POINT('Origin',(1.,-4.5,8.));
#23446=CARTESIAN_POINT('',(1.2,-4.5,8.6));
#23447=CARTESIAN_POINT('Origin',(1.2,-4.5,8.));
#23448=CARTESIAN_POINT('',(1.,-4.5,8.6));
#23449=CARTESIAN_POINT('',(1.,-4.5,8.6));
#23450=CARTESIAN_POINT('Origin',(1.,-4.5,8.));
#23451=CARTESIAN_POINT('Origin',(1.,-4.5,8.));
#23452=CARTESIAN_POINT('',(1.2,-4.5,8.9));
#23453=CARTESIAN_POINT('Origin',(1.2,-4.5,8.));
#23454=CARTESIAN_POINT('',(1.,-4.5,8.9));
#23455=CARTESIAN_POINT('',(1.,-4.5,8.9));
#23456=CARTESIAN_POINT('Origin',(1.,-4.5,8.));
#23457=CARTESIAN_POINT('Origin',(1.2,-4.5,8.));
#23458=CARTESIAN_POINT('Origin',(1.,-4.5,8.));
#23459=CARTESIAN_POINT('',(0.,0.,0.));
#23460=CARTESIAN_POINT('Origin',(-12.5,-4.5,8.));
#23461=CARTESIAN_POINT('',(-11.7,-4.5,8.6));
#23462=CARTESIAN_POINT('Origin',(-11.7,-4.5,8.));
#23463=CARTESIAN_POINT('',(-12.5,-4.5,8.6));
#23464=CARTESIAN_POINT('',(-12.5,-4.5,8.6));
#23465=CARTESIAN_POINT('Origin',(-12.5,-4.5,8.));
#23466=CARTESIAN_POINT('Origin',(-12.5,-4.5,8.));
#23467=CARTESIAN_POINT('',(-11.7,-4.5,10.));
#23468=CARTESIAN_POINT('Origin',(-11.7,-4.5,8.));
#23469=CARTESIAN_POINT('',(-12.5,-4.5,10.));
#23470=CARTESIAN_POINT('',(-12.5,-4.5,10.));
#23471=CARTESIAN_POINT('Origin',(-12.5,-4.5,8.));
#23472=CARTESIAN_POINT('Origin',(-11.7,-4.5,8.));
#23473=CARTESIAN_POINT('Origin',(-12.5,-4.5,8.));
#23474=CARTESIAN_POINT('',(0.,0.,0.));
#23475=CARTESIAN_POINT('Origin',(-14.5,-4.5,9.5));
#23476=CARTESIAN_POINT('',(-12.5,-4.5,9.9));
#23477=CARTESIAN_POINT('Origin',(-12.5,-4.5,9.5));
#23478=CARTESIAN_POINT('',(-14.5,-4.5,9.9));
#23479=CARTESIAN_POINT('',(-14.5,-4.5,9.9));
#23480=CARTESIAN_POINT('Origin',(-14.5,-4.5,9.5));
#23481=CARTESIAN_POINT('Origin',(-12.5,-4.5,9.5));
#23482=CARTESIAN_POINT('Origin',(-14.5,-4.5,9.5));
#23483=CARTESIAN_POINT('',(0.,0.,0.));
#23484=CARTESIAN_POINT('',(0.,0.,0.));
#23485=CARTESIAN_POINT('',(0.,0.,0.));
#23486=CARTESIAN_POINT('',(0.,0.,0.));
#23487=CARTESIAN_POINT('',(0.,0.,0.));
#23488=CARTESIAN_POINT('',(0.,0.,0.));
#23489=CARTESIAN_POINT('',(0.,0.,0.));
#23490=CARTESIAN_POINT('',(0.,0.,0.));
#23491=CARTESIAN_POINT('',(0.,0.,0.));
#23492=CARTESIAN_POINT('',(0.,0.,0.));
#23493=CARTESIAN_POINT('',(0.,0.,0.));
#23494=CARTESIAN_POINT('',(0.,0.,0.));
#23495=UNCERTAINTY_MEASURE_WITH_UNIT(LENGTH_MEASURE(0.001),#23729,
'DISTANCE_ACCURACY_VALUE',
'Maximum model space distance between geometric entities at asserted c
onnectivities');
#23496=UNCERTAINTY_MEASURE_WITH_UNIT(LENGTH_MEASURE(0.001),#23729,
'DISTANCE_ACCURACY_VALUE',
'Maximum model space distance between geometric entities at asserted c
onnectivities');
#23497=UNCERTAINTY_MEASURE_WITH_UNIT(LENGTH_MEASURE(0.001),#23729,
'DISTANCE_ACCURACY_VALUE',
'Maximum model space distance between geometric entities at asserted c
onnectivities');
#23498=UNCERTAINTY_MEASURE_WITH_UNIT(LENGTH_MEASURE(0.001),#23729,
'DISTANCE_ACCURACY_VALUE',
'Maximum model space distance between geometric entities at asserted c
onnectivities');
#23499=UNCERTAINTY_MEASURE_WITH_UNIT(LENGTH_MEASURE(0.001),#23729,
'DISTANCE_ACCURACY_VALUE',
'Maximum model space distance between geometric entities at asserted c
onnectivities');
#23500=UNCERTAINTY_MEASURE_WITH_UNIT(LENGTH_MEASURE(0.001),#23729,
'DISTANCE_ACCURACY_VALUE',
'Maximum model space distance between geometric entities at asserted c
onnectivities');
#23501=UNCERTAINTY_MEASURE_WITH_UNIT(LENGTH_MEASURE(0.001),#23729,
'DISTANCE_ACCURACY_VALUE',
'Maximum model space distance between geometric entities at asserted c
onnectivities');
#23502=UNCERTAINTY_MEASURE_WITH_UNIT(LENGTH_MEASURE(0.001),#23729,
'DISTANCE_ACCURACY_VALUE',
'Maximum model space distance between geometric entities at asserted c
onnectivities');
#23503=UNCERTAINTY_MEASURE_WITH_UNIT(LENGTH_MEASURE(0.001),#23729,
'DISTANCE_ACCURACY_VALUE',
'Maximum model space distance between geometric entities at asserted c
onnectivities');
#23504=UNCERTAINTY_MEASURE_WITH_UNIT(LENGTH_MEASURE(0.001),#23729,
'DISTANCE_ACCURACY_VALUE',
'Maximum model space distance between geometric entities at asserted c
onnectivities');
#23505=UNCERTAINTY_MEASURE_WITH_UNIT(LENGTH_MEASURE(0.001),#23729,
'DISTANCE_ACCURACY_VALUE',
'Maximum model space distance between geometric entities at asserted c
onnectivities');
#23506=UNCERTAINTY_MEASURE_WITH_UNIT(LENGTH_MEASURE(0.001),#23729,
'DISTANCE_ACCURACY_VALUE',
'Maximum model space distance between geometric entities at asserted c
onnectivities');
#23507=UNCERTAINTY_MEASURE_WITH_UNIT(LENGTH_MEASURE(0.001),#23729,
'DISTANCE_ACCURACY_VALUE',
'Maximum model space distance between geometric entities at asserted c
onnectivities');
#23508=UNCERTAINTY_MEASURE_WITH_UNIT(LENGTH_MEASURE(0.001),#23729,
'DISTANCE_ACCURACY_VALUE',
'Maximum model space distance between geometric entities at asserted c
onnectivities');
#23509=UNCERTAINTY_MEASURE_WITH_UNIT(LENGTH_MEASURE(0.001),#23729,
'DISTANCE_ACCURACY_VALUE',
'Maximum model space distance between geometric entities at asserted c
onnectivities');
#23510=UNCERTAINTY_MEASURE_WITH_UNIT(LENGTH_MEASURE(0.001),#23729,
'DISTANCE_ACCURACY_VALUE',
'Maximum model space distance between geometric entities at asserted c
onnectivities');
#23511=UNCERTAINTY_MEASURE_WITH_UNIT(LENGTH_MEASURE(0.001),#23729,
'DISTANCE_ACCURACY_VALUE',
'Maximum model space distance between geometric entities at asserted c
onnectivities');
#23512=UNCERTAINTY_MEASURE_WITH_UNIT(LENGTH_MEASURE(0.001),#23729,
'DISTANCE_ACCURACY_VALUE',
'Maximum model space distance between geometric entities at asserted c
onnectivities');
#23513=UNCERTAINTY_MEASURE_WITH_UNIT(LENGTH_MEASURE(0.001),#23729,
'DISTANCE_ACCURACY_VALUE',
'Maximum model space distance between geometric entities at asserted c
onnectivities');
#23514=UNCERTAINTY_MEASURE_WITH_UNIT(LENGTH_MEASURE(0.001),#23729,
'DISTANCE_ACCURACY_VALUE',
'Maximum model space distance between geometric entities at asserted c
onnectivities');
#23515=UNCERTAINTY_MEASURE_WITH_UNIT(LENGTH_MEASURE(0.001),#23729,
'DISTANCE_ACCURACY_VALUE',
'Maximum model space distance between geometric entities at asserted c
onnectivities');
#23516=UNCERTAINTY_MEASURE_WITH_UNIT(LENGTH_MEASURE(0.001),#23729,
'DISTANCE_ACCURACY_VALUE',
'Maximum model space distance between geometric entities at asserted c
onnectivities');
#23517=UNCERTAINTY_MEASURE_WITH_UNIT(LENGTH_MEASURE(0.001),#23729,
'DISTANCE_ACCURACY_VALUE',
'Maximum model space distance between geometric entities at asserted c
onnectivities');
#23518=UNCERTAINTY_MEASURE_WITH_UNIT(LENGTH_MEASURE(0.001),#23729,
'DISTANCE_ACCURACY_VALUE',
'Maximum model space distance between geometric entities at asserted c
onnectivities');
#23519=UNCERTAINTY_MEASURE_WITH_UNIT(LENGTH_MEASURE(0.001),#23729,
'DISTANCE_ACCURACY_VALUE',
'Maximum model space distance between geometric entities at asserted c
onnectivities');
#23520=UNCERTAINTY_MEASURE_WITH_UNIT(LENGTH_MEASURE(0.001),#23729,
'DISTANCE_ACCURACY_VALUE',
'Maximum model space distance between geometric entities at asserted c
onnectivities');
#23521=UNCERTAINTY_MEASURE_WITH_UNIT(LENGTH_MEASURE(0.001),#23729,
'DISTANCE_ACCURACY_VALUE',
'Maximum model space distance between geometric entities at asserted c
onnectivities');
#23522=UNCERTAINTY_MEASURE_WITH_UNIT(LENGTH_MEASURE(0.001),#23729,
'DISTANCE_ACCURACY_VALUE',
'Maximum model space distance between geometric entities at asserted c
onnectivities');
#23523=UNCERTAINTY_MEASURE_WITH_UNIT(LENGTH_MEASURE(0.001),#23729,
'DISTANCE_ACCURACY_VALUE',
'Maximum model space distance between geometric entities at asserted c
onnectivities');
#23524=UNCERTAINTY_MEASURE_WITH_UNIT(LENGTH_MEASURE(0.001),#23729,
'DISTANCE_ACCURACY_VALUE',
'Maximum model space distance between geometric entities at asserted c
onnectivities');
#23525=UNCERTAINTY_MEASURE_WITH_UNIT(LENGTH_MEASURE(0.001),#23729,
'DISTANCE_ACCURACY_VALUE',
'Maximum model space distance between geometric entities at asserted c
onnectivities');
#23526=UNCERTAINTY_MEASURE_WITH_UNIT(LENGTH_MEASURE(0.001),#23729,
'DISTANCE_ACCURACY_VALUE',
'Maximum model space distance between geometric entities at asserted c
onnectivities');
#23527=UNCERTAINTY_MEASURE_WITH_UNIT(LENGTH_MEASURE(0.001),#23729,
'DISTANCE_ACCURACY_VALUE',
'Maximum model space distance between geometric entities at asserted c
onnectivities');
#23528=UNCERTAINTY_MEASURE_WITH_UNIT(LENGTH_MEASURE(0.001),#23729,
'DISTANCE_ACCURACY_VALUE',
'Maximum model space distance between geometric entities at asserted c
onnectivities');
#23529=UNCERTAINTY_MEASURE_WITH_UNIT(LENGTH_MEASURE(0.001),#23729,
'DISTANCE_ACCURACY_VALUE',
'Maximum model space distance between geometric entities at asserted c
onnectivities');
#23530=UNCERTAINTY_MEASURE_WITH_UNIT(LENGTH_MEASURE(0.001),#23729,
'DISTANCE_ACCURACY_VALUE',
'Maximum model space distance between geometric entities at asserted c
onnectivities');
#23531=UNCERTAINTY_MEASURE_WITH_UNIT(LENGTH_MEASURE(0.001),#23729,
'DISTANCE_ACCURACY_VALUE',
'Maximum model space distance between geometric entities at asserted c
onnectivities');
#23532=UNCERTAINTY_MEASURE_WITH_UNIT(LENGTH_MEASURE(0.001),#23729,
'DISTANCE_ACCURACY_VALUE',
'Maximum model space distance between geometric entities at asserted c
onnectivities');
#23533=UNCERTAINTY_MEASURE_WITH_UNIT(LENGTH_MEASURE(0.001),#23729,
'DISTANCE_ACCURACY_VALUE',
'Maximum model space distance between geometric entities at asserted c
onnectivities');
#23534=UNCERTAINTY_MEASURE_WITH_UNIT(LENGTH_MEASURE(0.001),#23729,
'DISTANCE_ACCURACY_VALUE',
'Maximum model space distance between geometric entities at asserted c
onnectivities');
#23535=UNCERTAINTY_MEASURE_WITH_UNIT(LENGTH_MEASURE(0.001),#23729,
'DISTANCE_ACCURACY_VALUE',
'Maximum model space distance between geometric entities at asserted c
onnectivities');
#23536=UNCERTAINTY_MEASURE_WITH_UNIT(LENGTH_MEASURE(0.001),#23729,
'DISTANCE_ACCURACY_VALUE',
'Maximum model space distance between geometric entities at asserted c
onnectivities');
#23537=UNCERTAINTY_MEASURE_WITH_UNIT(LENGTH_MEASURE(0.001),#23729,
'DISTANCE_ACCURACY_VALUE',
'Maximum model space distance between geometric entities at asserted c
onnectivities');
#23538=UNCERTAINTY_MEASURE_WITH_UNIT(LENGTH_MEASURE(0.001),#23729,
'DISTANCE_ACCURACY_VALUE',
'Maximum model space distance between geometric entities at asserted c
onnectivities');
#23539=UNCERTAINTY_MEASURE_WITH_UNIT(LENGTH_MEASURE(0.001),#23729,
'DISTANCE_ACCURACY_VALUE',
'Maximum model space distance between geometric entities at asserted c
onnectivities');
#23540=UNCERTAINTY_MEASURE_WITH_UNIT(LENGTH_MEASURE(0.001),#23729,
'DISTANCE_ACCURACY_VALUE',
'Maximum model space distance between geometric entities at asserted c
onnectivities');
#23541=UNCERTAINTY_MEASURE_WITH_UNIT(LENGTH_MEASURE(0.001),#23729,
'DISTANCE_ACCURACY_VALUE',
'Maximum model space distance between geometric entities at asserted c
onnectivities');
#23542=UNCERTAINTY_MEASURE_WITH_UNIT(LENGTH_MEASURE(0.001),#23729,
'DISTANCE_ACCURACY_VALUE',
'Maximum model space distance between geometric entities at asserted c
onnectivities');
#23543=UNCERTAINTY_MEASURE_WITH_UNIT(LENGTH_MEASURE(0.001),#23729,
'DISTANCE_ACCURACY_VALUE',
'Maximum model space distance between geometric entities at asserted c
onnectivities');
#23544=UNCERTAINTY_MEASURE_WITH_UNIT(LENGTH_MEASURE(0.001),#23729,
'DISTANCE_ACCURACY_VALUE',
'Maximum model space distance between geometric entities at asserted c
onnectivities');
#23545=UNCERTAINTY_MEASURE_WITH_UNIT(LENGTH_MEASURE(0.001),#23729,
'DISTANCE_ACCURACY_VALUE',
'Maximum model space distance between geometric entities at asserted c
onnectivities');
#23546=UNCERTAINTY_MEASURE_WITH_UNIT(LENGTH_MEASURE(0.001),#23729,
'DISTANCE_ACCURACY_VALUE',
'Maximum model space distance between geometric entities at asserted c
onnectivities');
#23547=UNCERTAINTY_MEASURE_WITH_UNIT(LENGTH_MEASURE(0.001),#23729,
'DISTANCE_ACCURACY_VALUE',
'Maximum model space distance between geometric entities at asserted c
onnectivities');
#23548=UNCERTAINTY_MEASURE_WITH_UNIT(LENGTH_MEASURE(0.001),#23729,
'DISTANCE_ACCURACY_VALUE',
'Maximum model space distance between geometric entities at asserted c
onnectivities');
#23549=UNCERTAINTY_MEASURE_WITH_UNIT(LENGTH_MEASURE(0.001),#23729,
'DISTANCE_ACCURACY_VALUE',
'Maximum model space distance between geometric entities at asserted c
onnectivities');
#23550=UNCERTAINTY_MEASURE_WITH_UNIT(LENGTH_MEASURE(0.001),#23729,
'DISTANCE_ACCURACY_VALUE',
'Maximum model space distance between geometric entities at asserted c
onnectivities');
#23551=UNCERTAINTY_MEASURE_WITH_UNIT(LENGTH_MEASURE(0.001),#23729,
'DISTANCE_ACCURACY_VALUE',
'Maximum model space distance between geometric entities at asserted c
onnectivities');
#23552=UNCERTAINTY_MEASURE_WITH_UNIT(LENGTH_MEASURE(0.001),#23729,
'DISTANCE_ACCURACY_VALUE',
'Maximum model space distance between geometric entities at asserted c
onnectivities');
#23553=UNCERTAINTY_MEASURE_WITH_UNIT(LENGTH_MEASURE(0.001),#23729,
'DISTANCE_ACCURACY_VALUE',
'Maximum model space distance between geometric entities at asserted c
onnectivities');
#23554=UNCERTAINTY_MEASURE_WITH_UNIT(LENGTH_MEASURE(0.001),#23729,
'DISTANCE_ACCURACY_VALUE',
'Maximum model space distance between geometric entities at asserted c
onnectivities');
#23555=UNCERTAINTY_MEASURE_WITH_UNIT(LENGTH_MEASURE(0.001),#23729,
'DISTANCE_ACCURACY_VALUE',
'Maximum model space distance between geometric entities at asserted c
onnectivities');
#23556=UNCERTAINTY_MEASURE_WITH_UNIT(LENGTH_MEASURE(0.001),#23729,
'DISTANCE_ACCURACY_VALUE',
'Maximum model space distance between geometric entities at asserted c
onnectivities');
#23557=UNCERTAINTY_MEASURE_WITH_UNIT(LENGTH_MEASURE(0.001),#23729,
'DISTANCE_ACCURACY_VALUE',
'Maximum model space distance between geometric entities at asserted c
onnectivities');
#23558=UNCERTAINTY_MEASURE_WITH_UNIT(LENGTH_MEASURE(0.001),#23729,
'DISTANCE_ACCURACY_VALUE',
'Maximum model space distance between geometric entities at asserted c
onnectivities');
#23559=UNCERTAINTY_MEASURE_WITH_UNIT(LENGTH_MEASURE(0.001),#23729,
'DISTANCE_ACCURACY_VALUE',
'Maximum model space distance between geometric entities at asserted c
onnectivities');
#23560=UNCERTAINTY_MEASURE_WITH_UNIT(LENGTH_MEASURE(0.001),#23729,
'DISTANCE_ACCURACY_VALUE',
'Maximum model space distance between geometric entities at asserted c
onnectivities');
#23561=UNCERTAINTY_MEASURE_WITH_UNIT(LENGTH_MEASURE(0.001),#23729,
'DISTANCE_ACCURACY_VALUE',
'Maximum model space distance between geometric entities at asserted c
onnectivities');
#23562=UNCERTAINTY_MEASURE_WITH_UNIT(LENGTH_MEASURE(0.001),#23729,
'DISTANCE_ACCURACY_VALUE',
'Maximum model space distance between geometric entities at asserted c
onnectivities');
#23563=UNCERTAINTY_MEASURE_WITH_UNIT(LENGTH_MEASURE(0.001),#23729,
'DISTANCE_ACCURACY_VALUE',
'Maximum model space distance between geometric entities at asserted c
onnectivities');
#23564=UNCERTAINTY_MEASURE_WITH_UNIT(LENGTH_MEASURE(0.001),#23729,
'DISTANCE_ACCURACY_VALUE',
'Maximum model space distance between geometric entities at asserted c
onnectivities');
#23565=UNCERTAINTY_MEASURE_WITH_UNIT(LENGTH_MEASURE(0.001),#23729,
'DISTANCE_ACCURACY_VALUE',
'Maximum model space distance between geometric entities at asserted c
onnectivities');
#23566=UNCERTAINTY_MEASURE_WITH_UNIT(LENGTH_MEASURE(0.001),#23729,
'DISTANCE_ACCURACY_VALUE',
'Maximum model space distance between geometric entities at asserted c
onnectivities');
#23567=UNCERTAINTY_MEASURE_WITH_UNIT(LENGTH_MEASURE(0.001),#23729,
'DISTANCE_ACCURACY_VALUE',
'Maximum model space distance between geometric entities at asserted c
onnectivities');
#23568=UNCERTAINTY_MEASURE_WITH_UNIT(LENGTH_MEASURE(0.001),#23729,
'DISTANCE_ACCURACY_VALUE',
'Maximum model space distance between geometric entities at asserted c
onnectivities');
#23569=UNCERTAINTY_MEASURE_WITH_UNIT(LENGTH_MEASURE(0.001),#23729,
'DISTANCE_ACCURACY_VALUE',
'Maximum model space distance between geometric entities at asserted c
onnectivities');
#23570=UNCERTAINTY_MEASURE_WITH_UNIT(LENGTH_MEASURE(0.001),#23729,
'DISTANCE_ACCURACY_VALUE',
'Maximum model space distance between geometric entities at asserted c
onnectivities');
#23571=UNCERTAINTY_MEASURE_WITH_UNIT(LENGTH_MEASURE(0.001),#23729,
'DISTANCE_ACCURACY_VALUE',
'Maximum model space distance between geometric entities at asserted c
onnectivities');
#23572=UNCERTAINTY_MEASURE_WITH_UNIT(LENGTH_MEASURE(0.001),#23729,
'DISTANCE_ACCURACY_VALUE',
'Maximum model space distance between geometric entities at asserted c
onnectivities');
#23573=UNCERTAINTY_MEASURE_WITH_UNIT(LENGTH_MEASURE(0.001),#23729,
'DISTANCE_ACCURACY_VALUE',
'Maximum model space distance between geometric entities at asserted c
onnectivities');
#23574=UNCERTAINTY_MEASURE_WITH_UNIT(LENGTH_MEASURE(0.001),#23729,
'DISTANCE_ACCURACY_VALUE',
'Maximum model space distance between geometric entities at asserted c
onnectivities');
#23575=UNCERTAINTY_MEASURE_WITH_UNIT(LENGTH_MEASURE(0.001),#23729,
'DISTANCE_ACCURACY_VALUE',
'Maximum model space distance between geometric entities at asserted c
onnectivities');
#23576=UNCERTAINTY_MEASURE_WITH_UNIT(LENGTH_MEASURE(0.001),#23729,
'DISTANCE_ACCURACY_VALUE',
'Maximum model space distance between geometric entities at asserted c
onnectivities');
#23577=UNCERTAINTY_MEASURE_WITH_UNIT(LENGTH_MEASURE(0.001),#23729,
'DISTANCE_ACCURACY_VALUE',
'Maximum model space distance between geometric entities at asserted c
onnectivities');
#23578=UNCERTAINTY_MEASURE_WITH_UNIT(LENGTH_MEASURE(0.001),#23729,
'DISTANCE_ACCURACY_VALUE',
'Maximum model space distance between geometric entities at asserted c
onnectivities');
#23579=UNCERTAINTY_MEASURE_WITH_UNIT(LENGTH_MEASURE(0.001),#23729,
'DISTANCE_ACCURACY_VALUE',
'Maximum model space distance between geometric entities at asserted c
onnectivities');
#23580=UNCERTAINTY_MEASURE_WITH_UNIT(LENGTH_MEASURE(0.001),#23729,
'DISTANCE_ACCURACY_VALUE',
'Maximum model space distance between geometric entities at asserted c
onnectivities');
#23581=UNCERTAINTY_MEASURE_WITH_UNIT(LENGTH_MEASURE(0.001),#23729,
'DISTANCE_ACCURACY_VALUE',
'Maximum model space distance between geometric entities at asserted c
onnectivities');
#23582=UNCERTAINTY_MEASURE_WITH_UNIT(LENGTH_MEASURE(0.001),#23729,
'DISTANCE_ACCURACY_VALUE',
'Maximum model space distance between geometric entities at asserted c
onnectivities');
#23583=UNCERTAINTY_MEASURE_WITH_UNIT(LENGTH_MEASURE(0.001),#23729,
'DISTANCE_ACCURACY_VALUE',
'Maximum model space distance between geometric entities at asserted c
onnectivities');
#23584=UNCERTAINTY_MEASURE_WITH_UNIT(LENGTH_MEASURE(0.001),#23729,
'DISTANCE_ACCURACY_VALUE',
'Maximum model space distance between geometric entities at asserted c
onnectivities');
#23585=UNCERTAINTY_MEASURE_WITH_UNIT(LENGTH_MEASURE(0.001),#23729,
'DISTANCE_ACCURACY_VALUE',
'Maximum model space distance between geometric entities at asserted c
onnectivities');
#23586=UNCERTAINTY_MEASURE_WITH_UNIT(LENGTH_MEASURE(0.001),#23729,
'DISTANCE_ACCURACY_VALUE',
'Maximum model space distance between geometric entities at asserted c
onnectivities');
#23587=UNCERTAINTY_MEASURE_WITH_UNIT(LENGTH_MEASURE(0.001),#23729,
'DISTANCE_ACCURACY_VALUE',
'Maximum model space distance between geometric entities at asserted c
onnectivities');
#23588=UNCERTAINTY_MEASURE_WITH_UNIT(LENGTH_MEASURE(0.001),#23729,
'DISTANCE_ACCURACY_VALUE',
'Maximum model space distance between geometric entities at asserted c
onnectivities');
#23589=UNCERTAINTY_MEASURE_WITH_UNIT(LENGTH_MEASURE(0.001),#23729,
'DISTANCE_ACCURACY_VALUE',
'Maximum model space distance between geometric entities at asserted c
onnectivities');
#23590=UNCERTAINTY_MEASURE_WITH_UNIT(LENGTH_MEASURE(0.001),#23729,
'DISTANCE_ACCURACY_VALUE',
'Maximum model space distance between geometric entities at asserted c
onnectivities');
#23591=UNCERTAINTY_MEASURE_WITH_UNIT(LENGTH_MEASURE(0.001),#23729,
'DISTANCE_ACCURACY_VALUE',
'Maximum model space distance between geometric entities at asserted c
onnectivities');
#23592=UNCERTAINTY_MEASURE_WITH_UNIT(LENGTH_MEASURE(0.001),#23729,
'DISTANCE_ACCURACY_VALUE',
'Maximum model space distance between geometric entities at asserted c
onnectivities');
#23593=UNCERTAINTY_MEASURE_WITH_UNIT(LENGTH_MEASURE(0.001),#23729,
'DISTANCE_ACCURACY_VALUE',
'Maximum model space distance between geometric entities at asserted c
onnectivities');
#23594=UNCERTAINTY_MEASURE_WITH_UNIT(LENGTH_MEASURE(0.001),#23729,
'DISTANCE_ACCURACY_VALUE',
'Maximum model space distance between geometric entities at asserted c
onnectivities');
#23595=UNCERTAINTY_MEASURE_WITH_UNIT(LENGTH_MEASURE(0.001),#23729,
'DISTANCE_ACCURACY_VALUE',
'Maximum model space distance between geometric entities at asserted c
onnectivities');
#23596=UNCERTAINTY_MEASURE_WITH_UNIT(LENGTH_MEASURE(0.001),#23729,
'DISTANCE_ACCURACY_VALUE',
'Maximum model space distance between geometric entities at asserted c
onnectivities');
#23597=UNCERTAINTY_MEASURE_WITH_UNIT(LENGTH_MEASURE(0.001),#23729,
'DISTANCE_ACCURACY_VALUE',
'Maximum model space distance between geometric entities at asserted c
onnectivities');
#23598=UNCERTAINTY_MEASURE_WITH_UNIT(LENGTH_MEASURE(0.001),#23729,
'DISTANCE_ACCURACY_VALUE',
'Maximum model space distance between geometric entities at asserted c
onnectivities');
#23599=UNCERTAINTY_MEASURE_WITH_UNIT(LENGTH_MEASURE(0.001),#23729,
'DISTANCE_ACCURACY_VALUE',
'Maximum model space distance between geometric entities at asserted c
onnectivities');
#23600=UNCERTAINTY_MEASURE_WITH_UNIT(LENGTH_MEASURE(0.001),#23729,
'DISTANCE_ACCURACY_VALUE',
'Maximum model space distance between geometric entities at asserted c
onnectivities');
#23601=UNCERTAINTY_MEASURE_WITH_UNIT(LENGTH_MEASURE(0.001),#23729,
'DISTANCE_ACCURACY_VALUE',
'Maximum model space distance between geometric entities at asserted c
onnectivities');
#23602=UNCERTAINTY_MEASURE_WITH_UNIT(LENGTH_MEASURE(0.001),#23729,
'DISTANCE_ACCURACY_VALUE',
'Maximum model space distance between geometric entities at asserted c
onnectivities');
#23603=UNCERTAINTY_MEASURE_WITH_UNIT(LENGTH_MEASURE(0.001),#23729,
'DISTANCE_ACCURACY_VALUE',
'Maximum model space distance between geometric entities at asserted c
onnectivities');
#23604=UNCERTAINTY_MEASURE_WITH_UNIT(LENGTH_MEASURE(0.001),#23729,
'DISTANCE_ACCURACY_VALUE',
'Maximum model space distance between geometric entities at asserted c
onnectivities');
#23605=UNCERTAINTY_MEASURE_WITH_UNIT(LENGTH_MEASURE(0.001),#23729,
'DISTANCE_ACCURACY_VALUE',
'Maximum model space distance between geometric entities at asserted c
onnectivities');
#23606=UNCERTAINTY_MEASURE_WITH_UNIT(LENGTH_MEASURE(0.001),#23729,
'DISTANCE_ACCURACY_VALUE',
'Maximum model space distance between geometric entities at asserted c
onnectivities');
#23607=UNCERTAINTY_MEASURE_WITH_UNIT(LENGTH_MEASURE(0.001),#23729,
'DISTANCE_ACCURACY_VALUE',
'Maximum model space distance between geometric entities at asserted c
onnectivities');
#23608=UNCERTAINTY_MEASURE_WITH_UNIT(LENGTH_MEASURE(0.001),#23729,
'DISTANCE_ACCURACY_VALUE',
'Maximum model space distance between geometric entities at asserted c
onnectivities');
#23609=UNCERTAINTY_MEASURE_WITH_UNIT(LENGTH_MEASURE(0.001),#23729,
'DISTANCE_ACCURACY_VALUE',
'Maximum model space distance between geometric entities at asserted c
onnectivities');
#23610=UNCERTAINTY_MEASURE_WITH_UNIT(LENGTH_MEASURE(0.001),#23729,
'DISTANCE_ACCURACY_VALUE',
'Maximum model space distance between geometric entities at asserted c
onnectivities');
#23611=UNCERTAINTY_MEASURE_WITH_UNIT(LENGTH_MEASURE(0.001),#23729,
'DISTANCE_ACCURACY_VALUE',
'Maximum model space distance between geometric entities at asserted c
onnectivities');
#23612=(
GEOMETRIC_REPRESENTATION_CONTEXT(3)
GLOBAL_UNCERTAINTY_ASSIGNED_CONTEXT((#23495))
GLOBAL_UNIT_ASSIGNED_CONTEXT((#23729,#23731,#23732))
REPRESENTATION_CONTEXT('','3D')
);
#23613=(
GEOMETRIC_REPRESENTATION_CONTEXT(3)
GLOBAL_UNCERTAINTY_ASSIGNED_CONTEXT((#23496))
GLOBAL_UNIT_ASSIGNED_CONTEXT((#23729,#23731,#23732))
REPRESENTATION_CONTEXT('','3D')
);
#23614=(
GEOMETRIC_REPRESENTATION_CONTEXT(3)
GLOBAL_UNCERTAINTY_ASSIGNED_CONTEXT((#23497))
GLOBAL_UNIT_ASSIGNED_CONTEXT((#23729,#23731,#23732))
REPRESENTATION_CONTEXT('','3D')
);
#23615=(
GEOMETRIC_REPRESENTATION_CONTEXT(3)
GLOBAL_UNCERTAINTY_ASSIGNED_CONTEXT((#23498))
GLOBAL_UNIT_ASSIGNED_CONTEXT((#23729,#23731,#23732))
REPRESENTATION_CONTEXT('','3D')
);
#23616=(
GEOMETRIC_REPRESENTATION_CONTEXT(3)
GLOBAL_UNCERTAINTY_ASSIGNED_CONTEXT((#23499))
GLOBAL_UNIT_ASSIGNED_CONTEXT((#23729,#23731,#23732))
REPRESENTATION_CONTEXT('','3D')
);
#23617=(
GEOMETRIC_REPRESENTATION_CONTEXT(3)
GLOBAL_UNCERTAINTY_ASSIGNED_CONTEXT((#23500))
GLOBAL_UNIT_ASSIGNED_CONTEXT((#23729,#23731,#23732))
REPRESENTATION_CONTEXT('','3D')
);
#23618=(
GEOMETRIC_REPRESENTATION_CONTEXT(3)
GLOBAL_UNCERTAINTY_ASSIGNED_CONTEXT((#23501))
GLOBAL_UNIT_ASSIGNED_CONTEXT((#23729,#23731,#23732))
REPRESENTATION_CONTEXT('','3D')
);
#23619=(
GEOMETRIC_REPRESENTATION_CONTEXT(3)
GLOBAL_UNCERTAINTY_ASSIGNED_CONTEXT((#23502))
GLOBAL_UNIT_ASSIGNED_CONTEXT((#23729,#23731,#23732))
REPRESENTATION_CONTEXT('','3D')
);
#23620=(
GEOMETRIC_REPRESENTATION_CONTEXT(3)
GLOBAL_UNCERTAINTY_ASSIGNED_CONTEXT((#23503))
GLOBAL_UNIT_ASSIGNED_CONTEXT((#23729,#23731,#23732))
REPRESENTATION_CONTEXT('','3D')
);
#23621=(
GEOMETRIC_REPRESENTATION_CONTEXT(3)
GLOBAL_UNCERTAINTY_ASSIGNED_CONTEXT((#23504))
GLOBAL_UNIT_ASSIGNED_CONTEXT((#23729,#23731,#23732))
REPRESENTATION_CONTEXT('','3D')
);
#23622=(
GEOMETRIC_REPRESENTATION_CONTEXT(3)
GLOBAL_UNCERTAINTY_ASSIGNED_CONTEXT((#23505))
GLOBAL_UNIT_ASSIGNED_CONTEXT((#23729,#23731,#23732))
REPRESENTATION_CONTEXT('','3D')
);
#23623=(
GEOMETRIC_REPRESENTATION_CONTEXT(3)
GLOBAL_UNCERTAINTY_ASSIGNED_CONTEXT((#23506))
GLOBAL_UNIT_ASSIGNED_CONTEXT((#23729,#23731,#23732))
REPRESENTATION_CONTEXT('','3D')
);
#23624=(
GEOMETRIC_REPRESENTATION_CONTEXT(3)
GLOBAL_UNCERTAINTY_ASSIGNED_CONTEXT((#23507))
GLOBAL_UNIT_ASSIGNED_CONTEXT((#23729,#23731,#23732))
REPRESENTATION_CONTEXT('','3D')
);
#23625=(
GEOMETRIC_REPRESENTATION_CONTEXT(3)
GLOBAL_UNCERTAINTY_ASSIGNED_CONTEXT((#23508))
GLOBAL_UNIT_ASSIGNED_CONTEXT((#23729,#23731,#23732))
REPRESENTATION_CONTEXT('','3D')
);
#23626=(
GEOMETRIC_REPRESENTATION_CONTEXT(3)
GLOBAL_UNCERTAINTY_ASSIGNED_CONTEXT((#23509))
GLOBAL_UNIT_ASSIGNED_CONTEXT((#23729,#23731,#23732))
REPRESENTATION_CONTEXT('','3D')
);
#23627=(
GEOMETRIC_REPRESENTATION_CONTEXT(3)
GLOBAL_UNCERTAINTY_ASSIGNED_CONTEXT((#23510))
GLOBAL_UNIT_ASSIGNED_CONTEXT((#23729,#23731,#23732))
REPRESENTATION_CONTEXT('','3D')
);
#23628=(
GEOMETRIC_REPRESENTATION_CONTEXT(3)
GLOBAL_UNCERTAINTY_ASSIGNED_CONTEXT((#23511))
GLOBAL_UNIT_ASSIGNED_CONTEXT((#23729,#23731,#23732))
REPRESENTATION_CONTEXT('','3D')
);
#23629=(
GEOMETRIC_REPRESENTATION_CONTEXT(3)
GLOBAL_UNCERTAINTY_ASSIGNED_CONTEXT((#23512))
GLOBAL_UNIT_ASSIGNED_CONTEXT((#23729,#23731,#23732))
REPRESENTATION_CONTEXT('','3D')
);
#23630=(
GEOMETRIC_REPRESENTATION_CONTEXT(3)
GLOBAL_UNCERTAINTY_ASSIGNED_CONTEXT((#23513))
GLOBAL_UNIT_ASSIGNED_CONTEXT((#23729,#23731,#23732))
REPRESENTATION_CONTEXT('','3D')
);
#23631=(
GEOMETRIC_REPRESENTATION_CONTEXT(3)
GLOBAL_UNCERTAINTY_ASSIGNED_CONTEXT((#23514))
GLOBAL_UNIT_ASSIGNED_CONTEXT((#23729,#23731,#23732))
REPRESENTATION_CONTEXT('','3D')
);
#23632=(
GEOMETRIC_REPRESENTATION_CONTEXT(3)
GLOBAL_UNCERTAINTY_ASSIGNED_CONTEXT((#23515))
GLOBAL_UNIT_ASSIGNED_CONTEXT((#23729,#23731,#23732))
REPRESENTATION_CONTEXT('','3D')
);
#23633=(
GEOMETRIC_REPRESENTATION_CONTEXT(3)
GLOBAL_UNCERTAINTY_ASSIGNED_CONTEXT((#23516))
GLOBAL_UNIT_ASSIGNED_CONTEXT((#23729,#23731,#23732))
REPRESENTATION_CONTEXT('','3D')
);
#23634=(
GEOMETRIC_REPRESENTATION_CONTEXT(3)
GLOBAL_UNCERTAINTY_ASSIGNED_CONTEXT((#23517))
GLOBAL_UNIT_ASSIGNED_CONTEXT((#23729,#23731,#23732))
REPRESENTATION_CONTEXT('','3D')
);
#23635=(
GEOMETRIC_REPRESENTATION_CONTEXT(3)
GLOBAL_UNCERTAINTY_ASSIGNED_CONTEXT((#23518))
GLOBAL_UNIT_ASSIGNED_CONTEXT((#23729,#23731,#23732))
REPRESENTATION_CONTEXT('','3D')
);
#23636=(
GEOMETRIC_REPRESENTATION_CONTEXT(3)
GLOBAL_UNCERTAINTY_ASSIGNED_CONTEXT((#23519))
GLOBAL_UNIT_ASSIGNED_CONTEXT((#23729,#23731,#23732))
REPRESENTATION_CONTEXT('','3D')
);
#23637=(
GEOMETRIC_REPRESENTATION_CONTEXT(3)
GLOBAL_UNCERTAINTY_ASSIGNED_CONTEXT((#23520))
GLOBAL_UNIT_ASSIGNED_CONTEXT((#23729,#23731,#23732))
REPRESENTATION_CONTEXT('','3D')
);
#23638=(
GEOMETRIC_REPRESENTATION_CONTEXT(3)
GLOBAL_UNCERTAINTY_ASSIGNED_CONTEXT((#23521))
GLOBAL_UNIT_ASSIGNED_CONTEXT((#23729,#23731,#23732))
REPRESENTATION_CONTEXT('','3D')
);
#23639=(
GEOMETRIC_REPRESENTATION_CONTEXT(3)
GLOBAL_UNCERTAINTY_ASSIGNED_CONTEXT((#23522))
GLOBAL_UNIT_ASSIGNED_CONTEXT((#23729,#23731,#23732))
REPRESENTATION_CONTEXT('','3D')
);
#23640=(
GEOMETRIC_REPRESENTATION_CONTEXT(3)
GLOBAL_UNCERTAINTY_ASSIGNED_CONTEXT((#23523))
GLOBAL_UNIT_ASSIGNED_CONTEXT((#23729,#23731,#23732))
REPRESENTATION_CONTEXT('','3D')
);
#23641=(
GEOMETRIC_REPRESENTATION_CONTEXT(3)
GLOBAL_UNCERTAINTY_ASSIGNED_CONTEXT((#23524))
GLOBAL_UNIT_ASSIGNED_CONTEXT((#23729,#23731,#23732))
REPRESENTATION_CONTEXT('','3D')
);
#23642=(
GEOMETRIC_REPRESENTATION_CONTEXT(3)
GLOBAL_UNCERTAINTY_ASSIGNED_CONTEXT((#23525))
GLOBAL_UNIT_ASSIGNED_CONTEXT((#23729,#23731,#23732))
REPRESENTATION_CONTEXT('','3D')
);
#23643=(
GEOMETRIC_REPRESENTATION_CONTEXT(3)
GLOBAL_UNCERTAINTY_ASSIGNED_CONTEXT((#23526))
GLOBAL_UNIT_ASSIGNED_CONTEXT((#23729,#23731,#23732))
REPRESENTATION_CONTEXT('','3D')
);
#23644=(
GEOMETRIC_REPRESENTATION_CONTEXT(3)
GLOBAL_UNCERTAINTY_ASSIGNED_CONTEXT((#23527))
GLOBAL_UNIT_ASSIGNED_CONTEXT((#23729,#23731,#23732))
REPRESENTATION_CONTEXT('','3D')
);
#23645=(
GEOMETRIC_REPRESENTATION_CONTEXT(3)
GLOBAL_UNCERTAINTY_ASSIGNED_CONTEXT((#23528))
GLOBAL_UNIT_ASSIGNED_CONTEXT((#23729,#23731,#23732))
REPRESENTATION_CONTEXT('','3D')
);
#23646=(
GEOMETRIC_REPRESENTATION_CONTEXT(3)
GLOBAL_UNCERTAINTY_ASSIGNED_CONTEXT((#23529))
GLOBAL_UNIT_ASSIGNED_CONTEXT((#23729,#23731,#23732))
REPRESENTATION_CONTEXT('','3D')
);
#23647=(
GEOMETRIC_REPRESENTATION_CONTEXT(3)
GLOBAL_UNCERTAINTY_ASSIGNED_CONTEXT((#23530))
GLOBAL_UNIT_ASSIGNED_CONTEXT((#23729,#23731,#23732))
REPRESENTATION_CONTEXT('','3D')
);
#23648=(
GEOMETRIC_REPRESENTATION_CONTEXT(3)
GLOBAL_UNCERTAINTY_ASSIGNED_CONTEXT((#23531))
GLOBAL_UNIT_ASSIGNED_CONTEXT((#23729,#23731,#23732))
REPRESENTATION_CONTEXT('','3D')
);
#23649=(
GEOMETRIC_REPRESENTATION_CONTEXT(3)
GLOBAL_UNCERTAINTY_ASSIGNED_CONTEXT((#23532))
GLOBAL_UNIT_ASSIGNED_CONTEXT((#23729,#23731,#23732))
REPRESENTATION_CONTEXT('','3D')
);
#23650=(
GEOMETRIC_REPRESENTATION_CONTEXT(3)
GLOBAL_UNCERTAINTY_ASSIGNED_CONTEXT((#23533))
GLOBAL_UNIT_ASSIGNED_CONTEXT((#23729,#23731,#23732))
REPRESENTATION_CONTEXT('','3D')
);
#23651=(
GEOMETRIC_REPRESENTATION_CONTEXT(3)
GLOBAL_UNCERTAINTY_ASSIGNED_CONTEXT((#23534))
GLOBAL_UNIT_ASSIGNED_CONTEXT((#23729,#23731,#23732))
REPRESENTATION_CONTEXT('','3D')
);
#23652=(
GEOMETRIC_REPRESENTATION_CONTEXT(3)
GLOBAL_UNCERTAINTY_ASSIGNED_CONTEXT((#23535))
GLOBAL_UNIT_ASSIGNED_CONTEXT((#23729,#23731,#23732))
REPRESENTATION_CONTEXT('','3D')
);
#23653=(
GEOMETRIC_REPRESENTATION_CONTEXT(3)
GLOBAL_UNCERTAINTY_ASSIGNED_CONTEXT((#23536))
GLOBAL_UNIT_ASSIGNED_CONTEXT((#23729,#23731,#23732))
REPRESENTATION_CONTEXT('','3D')
);
#23654=(
GEOMETRIC_REPRESENTATION_CONTEXT(3)
GLOBAL_UNCERTAINTY_ASSIGNED_CONTEXT((#23537))
GLOBAL_UNIT_ASSIGNED_CONTEXT((#23729,#23731,#23732))
REPRESENTATION_CONTEXT('','3D')
);
#23655=(
GEOMETRIC_REPRESENTATION_CONTEXT(3)
GLOBAL_UNCERTAINTY_ASSIGNED_CONTEXT((#23538))
GLOBAL_UNIT_ASSIGNED_CONTEXT((#23729,#23731,#23732))
REPRESENTATION_CONTEXT('','3D')
);
#23656=(
GEOMETRIC_REPRESENTATION_CONTEXT(3)
GLOBAL_UNCERTAINTY_ASSIGNED_CONTEXT((#23539))
GLOBAL_UNIT_ASSIGNED_CONTEXT((#23729,#23731,#23732))
REPRESENTATION_CONTEXT('','3D')
);
#23657=(
GEOMETRIC_REPRESENTATION_CONTEXT(3)
GLOBAL_UNCERTAINTY_ASSIGNED_CONTEXT((#23540))
GLOBAL_UNIT_ASSIGNED_CONTEXT((#23729,#23731,#23732))
REPRESENTATION_CONTEXT('','3D')
);
#23658=(
GEOMETRIC_REPRESENTATION_CONTEXT(3)
GLOBAL_UNCERTAINTY_ASSIGNED_CONTEXT((#23541))
GLOBAL_UNIT_ASSIGNED_CONTEXT((#23729,#23731,#23732))
REPRESENTATION_CONTEXT('','3D')
);
#23659=(
GEOMETRIC_REPRESENTATION_CONTEXT(3)
GLOBAL_UNCERTAINTY_ASSIGNED_CONTEXT((#23542))
GLOBAL_UNIT_ASSIGNED_CONTEXT((#23729,#23731,#23732))
REPRESENTATION_CONTEXT('','3D')
);
#23660=(
GEOMETRIC_REPRESENTATION_CONTEXT(3)
GLOBAL_UNCERTAINTY_ASSIGNED_CONTEXT((#23543))
GLOBAL_UNIT_ASSIGNED_CONTEXT((#23729,#23731,#23732))
REPRESENTATION_CONTEXT('','3D')
);
#23661=(
GEOMETRIC_REPRESENTATION_CONTEXT(3)
GLOBAL_UNCERTAINTY_ASSIGNED_CONTEXT((#23544))
GLOBAL_UNIT_ASSIGNED_CONTEXT((#23729,#23731,#23732))
REPRESENTATION_CONTEXT('','3D')
);
#23662=(
GEOMETRIC_REPRESENTATION_CONTEXT(3)
GLOBAL_UNCERTAINTY_ASSIGNED_CONTEXT((#23545))
GLOBAL_UNIT_ASSIGNED_CONTEXT((#23729,#23731,#23732))
REPRESENTATION_CONTEXT('','3D')
);
#23663=(
GEOMETRIC_REPRESENTATION_CONTEXT(3)
GLOBAL_UNCERTAINTY_ASSIGNED_CONTEXT((#23546))
GLOBAL_UNIT_ASSIGNED_CONTEXT((#23729,#23731,#23732))
REPRESENTATION_CONTEXT('','3D')
);
#23664=(
GEOMETRIC_REPRESENTATION_CONTEXT(3)
GLOBAL_UNCERTAINTY_ASSIGNED_CONTEXT((#23547))
GLOBAL_UNIT_ASSIGNED_CONTEXT((#23729,#23731,#23732))
REPRESENTATION_CONTEXT('','3D')
);
#23665=(
GEOMETRIC_REPRESENTATION_CONTEXT(3)
GLOBAL_UNCERTAINTY_ASSIGNED_CONTEXT((#23548))
GLOBAL_UNIT_ASSIGNED_CONTEXT((#23729,#23731,#23732))
REPRESENTATION_CONTEXT('','3D')
);
#23666=(
GEOMETRIC_REPRESENTATION_CONTEXT(3)
GLOBAL_UNCERTAINTY_ASSIGNED_CONTEXT((#23549))
GLOBAL_UNIT_ASSIGNED_CONTEXT((#23729,#23731,#23732))
REPRESENTATION_CONTEXT('','3D')
);
#23667=(
GEOMETRIC_REPRESENTATION_CONTEXT(3)
GLOBAL_UNCERTAINTY_ASSIGNED_CONTEXT((#23550))
GLOBAL_UNIT_ASSIGNED_CONTEXT((#23729,#23731,#23732))
REPRESENTATION_CONTEXT('','3D')
);
#23668=(
GEOMETRIC_REPRESENTATION_CONTEXT(3)
GLOBAL_UNCERTAINTY_ASSIGNED_CONTEXT((#23551))
GLOBAL_UNIT_ASSIGNED_CONTEXT((#23729,#23731,#23732))
REPRESENTATION_CONTEXT('','3D')
);
#23669=(
GEOMETRIC_REPRESENTATION_CONTEXT(3)
GLOBAL_UNCERTAINTY_ASSIGNED_CONTEXT((#23552))
GLOBAL_UNIT_ASSIGNED_CONTEXT((#23729,#23731,#23732))
REPRESENTATION_CONTEXT('','3D')
);
#23670=(
GEOMETRIC_REPRESENTATION_CONTEXT(3)
GLOBAL_UNCERTAINTY_ASSIGNED_CONTEXT((#23553))
GLOBAL_UNIT_ASSIGNED_CONTEXT((#23729,#23731,#23732))
REPRESENTATION_CONTEXT('','3D')
);
#23671=(
GEOMETRIC_REPRESENTATION_CONTEXT(3)
GLOBAL_UNCERTAINTY_ASSIGNED_CONTEXT((#23554))
GLOBAL_UNIT_ASSIGNED_CONTEXT((#23729,#23731,#23732))
REPRESENTATION_CONTEXT('','3D')
);
#23672=(
GEOMETRIC_REPRESENTATION_CONTEXT(3)
GLOBAL_UNCERTAINTY_ASSIGNED_CONTEXT((#23555))
GLOBAL_UNIT_ASSIGNED_CONTEXT((#23729,#23731,#23732))
REPRESENTATION_CONTEXT('','3D')
);
#23673=(
GEOMETRIC_REPRESENTATION_CONTEXT(3)
GLOBAL_UNCERTAINTY_ASSIGNED_CONTEXT((#23556))
GLOBAL_UNIT_ASSIGNED_CONTEXT((#23729,#23731,#23732))
REPRESENTATION_CONTEXT('','3D')
);
#23674=(
GEOMETRIC_REPRESENTATION_CONTEXT(3)
GLOBAL_UNCERTAINTY_ASSIGNED_CONTEXT((#23557))
GLOBAL_UNIT_ASSIGNED_CONTEXT((#23729,#23731,#23732))
REPRESENTATION_CONTEXT('','3D')
);
#23675=(
GEOMETRIC_REPRESENTATION_CONTEXT(3)
GLOBAL_UNCERTAINTY_ASSIGNED_CONTEXT((#23558))
GLOBAL_UNIT_ASSIGNED_CONTEXT((#23729,#23731,#23732))
REPRESENTATION_CONTEXT('','3D')
);
#23676=(
GEOMETRIC_REPRESENTATION_CONTEXT(3)
GLOBAL_UNCERTAINTY_ASSIGNED_CONTEXT((#23559))
GLOBAL_UNIT_ASSIGNED_CONTEXT((#23729,#23731,#23732))
REPRESENTATION_CONTEXT('','3D')
);
#23677=(
GEOMETRIC_REPRESENTATION_CONTEXT(3)
GLOBAL_UNCERTAINTY_ASSIGNED_CONTEXT((#23560))
GLOBAL_UNIT_ASSIGNED_CONTEXT((#23729,#23731,#23732))
REPRESENTATION_CONTEXT('','3D')
);
#23678=(
GEOMETRIC_REPRESENTATION_CONTEXT(3)
GLOBAL_UNCERTAINTY_ASSIGNED_CONTEXT((#23561))
GLOBAL_UNIT_ASSIGNED_CONTEXT((#23729,#23731,#23732))
REPRESENTATION_CONTEXT('','3D')
);
#23679=(
GEOMETRIC_REPRESENTATION_CONTEXT(3)
GLOBAL_UNCERTAINTY_ASSIGNED_CONTEXT((#23562))
GLOBAL_UNIT_ASSIGNED_CONTEXT((#23729,#23731,#23732))
REPRESENTATION_CONTEXT('','3D')
);
#23680=(
GEOMETRIC_REPRESENTATION_CONTEXT(3)
GLOBAL_UNCERTAINTY_ASSIGNED_CONTEXT((#23563))
GLOBAL_UNIT_ASSIGNED_CONTEXT((#23729,#23731,#23732))
REPRESENTATION_CONTEXT('','3D')
);
#23681=(
GEOMETRIC_REPRESENTATION_CONTEXT(3)
GLOBAL_UNCERTAINTY_ASSIGNED_CONTEXT((#23564))
GLOBAL_UNIT_ASSIGNED_CONTEXT((#23729,#23731,#23732))
REPRESENTATION_CONTEXT('','3D')
);
#23682=(
GEOMETRIC_REPRESENTATION_CONTEXT(3)
GLOBAL_UNCERTAINTY_ASSIGNED_CONTEXT((#23565))
GLOBAL_UNIT_ASSIGNED_CONTEXT((#23729,#23731,#23732))
REPRESENTATION_CONTEXT('','3D')
);
#23683=(
GEOMETRIC_REPRESENTATION_CONTEXT(3)
GLOBAL_UNCERTAINTY_ASSIGNED_CONTEXT((#23566))
GLOBAL_UNIT_ASSIGNED_CONTEXT((#23729,#23731,#23732))
REPRESENTATION_CONTEXT('','3D')
);
#23684=(
GEOMETRIC_REPRESENTATION_CONTEXT(3)
GLOBAL_UNCERTAINTY_ASSIGNED_CONTEXT((#23567))
GLOBAL_UNIT_ASSIGNED_CONTEXT((#23729,#23731,#23732))
REPRESENTATION_CONTEXT('','3D')
);
#23685=(
GEOMETRIC_REPRESENTATION_CONTEXT(3)
GLOBAL_UNCERTAINTY_ASSIGNED_CONTEXT((#23568))
GLOBAL_UNIT_ASSIGNED_CONTEXT((#23729,#23731,#23732))
REPRESENTATION_CONTEXT('','3D')
);
#23686=(
GEOMETRIC_REPRESENTATION_CONTEXT(3)
GLOBAL_UNCERTAINTY_ASSIGNED_CONTEXT((#23569))
GLOBAL_UNIT_ASSIGNED_CONTEXT((#23729,#23731,#23732))
REPRESENTATION_CONTEXT('','3D')
);
#23687=(
GEOMETRIC_REPRESENTATION_CONTEXT(3)
GLOBAL_UNCERTAINTY_ASSIGNED_CONTEXT((#23570))
GLOBAL_UNIT_ASSIGNED_CONTEXT((#23729,#23731,#23732))
REPRESENTATION_CONTEXT('','3D')
);
#23688=(
GEOMETRIC_REPRESENTATION_CONTEXT(3)
GLOBAL_UNCERTAINTY_ASSIGNED_CONTEXT((#23571))
GLOBAL_UNIT_ASSIGNED_CONTEXT((#23729,#23731,#23732))
REPRESENTATION_CONTEXT('','3D')
);
#23689=(
GEOMETRIC_REPRESENTATION_CONTEXT(3)
GLOBAL_UNCERTAINTY_ASSIGNED_CONTEXT((#23572))
GLOBAL_UNIT_ASSIGNED_CONTEXT((#23729,#23731,#23732))
REPRESENTATION_CONTEXT('','3D')
);
#23690=(
GEOMETRIC_REPRESENTATION_CONTEXT(3)
GLOBAL_UNCERTAINTY_ASSIGNED_CONTEXT((#23573))
GLOBAL_UNIT_ASSIGNED_CONTEXT((#23729,#23731,#23732))
REPRESENTATION_CONTEXT('','3D')
);
#23691=(
GEOMETRIC_REPRESENTATION_CONTEXT(3)
GLOBAL_UNCERTAINTY_ASSIGNED_CONTEXT((#23574))
GLOBAL_UNIT_ASSIGNED_CONTEXT((#23729,#23731,#23732))
REPRESENTATION_CONTEXT('','3D')
);
#23692=(
GEOMETRIC_REPRESENTATION_CONTEXT(3)
GLOBAL_UNCERTAINTY_ASSIGNED_CONTEXT((#23575))
GLOBAL_UNIT_ASSIGNED_CONTEXT((#23729,#23731,#23732))
REPRESENTATION_CONTEXT('','3D')
);
#23693=(
GEOMETRIC_REPRESENTATION_CONTEXT(3)
GLOBAL_UNCERTAINTY_ASSIGNED_CONTEXT((#23576))
GLOBAL_UNIT_ASSIGNED_CONTEXT((#23729,#23731,#23732))
REPRESENTATION_CONTEXT('','3D')
);
#23694=(
GEOMETRIC_REPRESENTATION_CONTEXT(3)
GLOBAL_UNCERTAINTY_ASSIGNED_CONTEXT((#23577))
GLOBAL_UNIT_ASSIGNED_CONTEXT((#23729,#23731,#23732))
REPRESENTATION_CONTEXT('','3D')
);
#23695=(
GEOMETRIC_REPRESENTATION_CONTEXT(3)
GLOBAL_UNCERTAINTY_ASSIGNED_CONTEXT((#23578))
GLOBAL_UNIT_ASSIGNED_CONTEXT((#23729,#23731,#23732))
REPRESENTATION_CONTEXT('','3D')
);
#23696=(
GEOMETRIC_REPRESENTATION_CONTEXT(3)
GLOBAL_UNCERTAINTY_ASSIGNED_CONTEXT((#23579))
GLOBAL_UNIT_ASSIGNED_CONTEXT((#23729,#23731,#23732))
REPRESENTATION_CONTEXT('','3D')
);
#23697=(
GEOMETRIC_REPRESENTATION_CONTEXT(3)
GLOBAL_UNCERTAINTY_ASSIGNED_CONTEXT((#23580))
GLOBAL_UNIT_ASSIGNED_CONTEXT((#23729,#23731,#23732))
REPRESENTATION_CONTEXT('','3D')
);
#23698=(
GEOMETRIC_REPRESENTATION_CONTEXT(3)
GLOBAL_UNCERTAINTY_ASSIGNED_CONTEXT((#23581))
GLOBAL_UNIT_ASSIGNED_CONTEXT((#23729,#23731,#23732))
REPRESENTATION_CONTEXT('','3D')
);
#23699=(
GEOMETRIC_REPRESENTATION_CONTEXT(3)
GLOBAL_UNCERTAINTY_ASSIGNED_CONTEXT((#23582))
GLOBAL_UNIT_ASSIGNED_CONTEXT((#23729,#23731,#23732))
REPRESENTATION_CONTEXT('','3D')
);
#23700=(
GEOMETRIC_REPRESENTATION_CONTEXT(3)
GLOBAL_UNCERTAINTY_ASSIGNED_CONTEXT((#23583))
GLOBAL_UNIT_ASSIGNED_CONTEXT((#23729,#23731,#23732))
REPRESENTATION_CONTEXT('','3D')
);
#23701=(
GEOMETRIC_REPRESENTATION_CONTEXT(3)
GLOBAL_UNCERTAINTY_ASSIGNED_CONTEXT((#23584))
GLOBAL_UNIT_ASSIGNED_CONTEXT((#23729,#23731,#23732))
REPRESENTATION_CONTEXT('','3D')
);
#23702=(
GEOMETRIC_REPRESENTATION_CONTEXT(3)
GLOBAL_UNCERTAINTY_ASSIGNED_CONTEXT((#23585))
GLOBAL_UNIT_ASSIGNED_CONTEXT((#23729,#23731,#23732))
REPRESENTATION_CONTEXT('','3D')
);
#23703=(
GEOMETRIC_REPRESENTATION_CONTEXT(3)
GLOBAL_UNCERTAINTY_ASSIGNED_CONTEXT((#23586))
GLOBAL_UNIT_ASSIGNED_CONTEXT((#23729,#23731,#23732))
REPRESENTATION_CONTEXT('','3D')
);
#23704=(
GEOMETRIC_REPRESENTATION_CONTEXT(3)
GLOBAL_UNCERTAINTY_ASSIGNED_CONTEXT((#23587))
GLOBAL_UNIT_ASSIGNED_CONTEXT((#23729,#23731,#23732))
REPRESENTATION_CONTEXT('','3D')
);
#23705=(
GEOMETRIC_REPRESENTATION_CONTEXT(3)
GLOBAL_UNCERTAINTY_ASSIGNED_CONTEXT((#23588))
GLOBAL_UNIT_ASSIGNED_CONTEXT((#23729,#23731,#23732))
REPRESENTATION_CONTEXT('','3D')
);
#23706=(
GEOMETRIC_REPRESENTATION_CONTEXT(3)
GLOBAL_UNCERTAINTY_ASSIGNED_CONTEXT((#23589))
GLOBAL_UNIT_ASSIGNED_CONTEXT((#23729,#23731,#23732))
REPRESENTATION_CONTEXT('','3D')
);
#23707=(
GEOMETRIC_REPRESENTATION_CONTEXT(3)
GLOBAL_UNCERTAINTY_ASSIGNED_CONTEXT((#23590))
GLOBAL_UNIT_ASSIGNED_CONTEXT((#23729,#23731,#23732))
REPRESENTATION_CONTEXT('','3D')
);
#23708=(
GEOMETRIC_REPRESENTATION_CONTEXT(3)
GLOBAL_UNCERTAINTY_ASSIGNED_CONTEXT((#23591))
GLOBAL_UNIT_ASSIGNED_CONTEXT((#23729,#23731,#23732))
REPRESENTATION_CONTEXT('','3D')
);
#23709=(
GEOMETRIC_REPRESENTATION_CONTEXT(3)
GLOBAL_UNCERTAINTY_ASSIGNED_CONTEXT((#23592))
GLOBAL_UNIT_ASSIGNED_CONTEXT((#23729,#23731,#23732))
REPRESENTATION_CONTEXT('','3D')
);
#23710=(
GEOMETRIC_REPRESENTATION_CONTEXT(3)
GLOBAL_UNCERTAINTY_ASSIGNED_CONTEXT((#23593))
GLOBAL_UNIT_ASSIGNED_CONTEXT((#23729,#23731,#23732))
REPRESENTATION_CONTEXT('','3D')
);
#23711=(
GEOMETRIC_REPRESENTATION_CONTEXT(3)
GLOBAL_UNCERTAINTY_ASSIGNED_CONTEXT((#23594))
GLOBAL_UNIT_ASSIGNED_CONTEXT((#23729,#23731,#23732))
REPRESENTATION_CONTEXT('','3D')
);
#23712=(
GEOMETRIC_REPRESENTATION_CONTEXT(3)
GLOBAL_UNCERTAINTY_ASSIGNED_CONTEXT((#23595))
GLOBAL_UNIT_ASSIGNED_CONTEXT((#23729,#23731,#23732))
REPRESENTATION_CONTEXT('','3D')
);
#23713=(
GEOMETRIC_REPRESENTATION_CONTEXT(3)
GLOBAL_UNCERTAINTY_ASSIGNED_CONTEXT((#23596))
GLOBAL_UNIT_ASSIGNED_CONTEXT((#23729,#23731,#23732))
REPRESENTATION_CONTEXT('','3D')
);
#23714=(
GEOMETRIC_REPRESENTATION_CONTEXT(3)
GLOBAL_UNCERTAINTY_ASSIGNED_CONTEXT((#23597))
GLOBAL_UNIT_ASSIGNED_CONTEXT((#23729,#23731,#23732))
REPRESENTATION_CONTEXT('','3D')
);
#23715=(
GEOMETRIC_REPRESENTATION_CONTEXT(3)
GLOBAL_UNCERTAINTY_ASSIGNED_CONTEXT((#23598))
GLOBAL_UNIT_ASSIGNED_CONTEXT((#23729,#23731,#23732))
REPRESENTATION_CONTEXT('','3D')
);
#23716=(
GEOMETRIC_REPRESENTATION_CONTEXT(3)
GLOBAL_UNCERTAINTY_ASSIGNED_CONTEXT((#23599))
GLOBAL_UNIT_ASSIGNED_CONTEXT((#23729,#23731,#23732))
REPRESENTATION_CONTEXT('','3D')
);
#23717=(
GEOMETRIC_REPRESENTATION_CONTEXT(3)
GLOBAL_UNCERTAINTY_ASSIGNED_CONTEXT((#23600))
GLOBAL_UNIT_ASSIGNED_CONTEXT((#23729,#23731,#23732))
REPRESENTATION_CONTEXT('','3D')
);
#23718=(
GEOMETRIC_REPRESENTATION_CONTEXT(3)
GLOBAL_UNCERTAINTY_ASSIGNED_CONTEXT((#23601))
GLOBAL_UNIT_ASSIGNED_CONTEXT((#23729,#23731,#23732))
REPRESENTATION_CONTEXT('','3D')
);
#23719=(
GEOMETRIC_REPRESENTATION_CONTEXT(3)
GLOBAL_UNCERTAINTY_ASSIGNED_CONTEXT((#23602))
GLOBAL_UNIT_ASSIGNED_CONTEXT((#23729,#23731,#23732))
REPRESENTATION_CONTEXT('','3D')
);
#23720=(
GEOMETRIC_REPRESENTATION_CONTEXT(3)
GLOBAL_UNCERTAINTY_ASSIGNED_CONTEXT((#23603))
GLOBAL_UNIT_ASSIGNED_CONTEXT((#23729,#23731,#23732))
REPRESENTATION_CONTEXT('','3D')
);
#23721=(
GEOMETRIC_REPRESENTATION_CONTEXT(3)
GLOBAL_UNCERTAINTY_ASSIGNED_CONTEXT((#23604))
GLOBAL_UNIT_ASSIGNED_CONTEXT((#23729,#23731,#23732))
REPRESENTATION_CONTEXT('','3D')
);
#23722=(
GEOMETRIC_REPRESENTATION_CONTEXT(3)
GLOBAL_UNCERTAINTY_ASSIGNED_CONTEXT((#23605))
GLOBAL_UNIT_ASSIGNED_CONTEXT((#23729,#23731,#23732))
REPRESENTATION_CONTEXT('','3D')
);
#23723=(
GEOMETRIC_REPRESENTATION_CONTEXT(3)
GLOBAL_UNCERTAINTY_ASSIGNED_CONTEXT((#23606))
GLOBAL_UNIT_ASSIGNED_CONTEXT((#23729,#23731,#23732))
REPRESENTATION_CONTEXT('','3D')
);
#23724=(
GEOMETRIC_REPRESENTATION_CONTEXT(3)
GLOBAL_UNCERTAINTY_ASSIGNED_CONTEXT((#23607))
GLOBAL_UNIT_ASSIGNED_CONTEXT((#23729,#23731,#23732))
REPRESENTATION_CONTEXT('','3D')
);
#23725=(
GEOMETRIC_REPRESENTATION_CONTEXT(3)
GLOBAL_UNCERTAINTY_ASSIGNED_CONTEXT((#23608))
GLOBAL_UNIT_ASSIGNED_CONTEXT((#23729,#23731,#23732))
REPRESENTATION_CONTEXT('','3D')
);
#23726=(
GEOMETRIC_REPRESENTATION_CONTEXT(3)
GLOBAL_UNCERTAINTY_ASSIGNED_CONTEXT((#23609))
GLOBAL_UNIT_ASSIGNED_CONTEXT((#23729,#23731,#23732))
REPRESENTATION_CONTEXT('','3D')
);
#23727=(
GEOMETRIC_REPRESENTATION_CONTEXT(3)
GLOBAL_UNCERTAINTY_ASSIGNED_CONTEXT((#23610))
GLOBAL_UNIT_ASSIGNED_CONTEXT((#23729,#23731,#23732))
REPRESENTATION_CONTEXT('','3D')
);
#23728=(
GEOMETRIC_REPRESENTATION_CONTEXT(3)
GLOBAL_UNCERTAINTY_ASSIGNED_CONTEXT((#23611))
GLOBAL_UNIT_ASSIGNED_CONTEXT((#23729,#23731,#23732))
REPRESENTATION_CONTEXT('','3D')
);
#23729=(
LENGTH_UNIT()
NAMED_UNIT(*)
SI_UNIT(.CENTI.,.METRE.)
);
#23730=(
LENGTH_UNIT()
NAMED_UNIT(*)
SI_UNIT($,.METRE.)
);
#23731=(
NAMED_UNIT(*)
PLANE_ANGLE_UNIT()
SI_UNIT($,.RADIAN.)
);
#23732=(
NAMED_UNIT(*)
SI_UNIT($,.STERADIAN.)
SOLID_ANGLE_UNIT()
);
#23733=SHAPE_DEFINITION_REPRESENTATION(#23849,#24112);
#23734=SHAPE_DEFINITION_REPRESENTATION(#23850,#24113);
#23735=SHAPE_DEFINITION_REPRESENTATION(#23851,#24114);
#23736=SHAPE_DEFINITION_REPRESENTATION(#23852,#24115);
#23737=SHAPE_DEFINITION_REPRESENTATION(#23853,#24116);
#23738=SHAPE_DEFINITION_REPRESENTATION(#23854,#24117);
#23739=SHAPE_DEFINITION_REPRESENTATION(#23855,#24118);
#23740=SHAPE_DEFINITION_REPRESENTATION(#23856,#24119);
#23741=SHAPE_DEFINITION_REPRESENTATION(#23857,#24120);
#23742=SHAPE_DEFINITION_REPRESENTATION(#23858,#24121);
#23743=SHAPE_DEFINITION_REPRESENTATION(#23859,#24122);
#23744=SHAPE_DEFINITION_REPRESENTATION(#23860,#24123);
#23745=SHAPE_DEFINITION_REPRESENTATION(#23861,#24124);
#23746=SHAPE_DEFINITION_REPRESENTATION(#23862,#24125);
#23747=SHAPE_DEFINITION_REPRESENTATION(#23863,#24126);
#23748=SHAPE_DEFINITION_REPRESENTATION(#23864,#24127);
#23749=SHAPE_DEFINITION_REPRESENTATION(#23865,#24128);
#23750=SHAPE_DEFINITION_REPRESENTATION(#23866,#24129);
#23751=SHAPE_DEFINITION_REPRESENTATION(#23867,#24130);
#23752=SHAPE_DEFINITION_REPRESENTATION(#23868,#24131);
#23753=SHAPE_DEFINITION_REPRESENTATION(#23869,#24132);
#23754=SHAPE_DEFINITION_REPRESENTATION(#23870,#24133);
#23755=SHAPE_DEFINITION_REPRESENTATION(#23871,#24134);
#23756=SHAPE_DEFINITION_REPRESENTATION(#23872,#24135);
#23757=SHAPE_DEFINITION_REPRESENTATION(#23873,#24136);
#23758=SHAPE_DEFINITION_REPRESENTATION(#23874,#24137);
#23759=SHAPE_DEFINITION_REPRESENTATION(#23875,#24138);
#23760=SHAPE_DEFINITION_REPRESENTATION(#23876,#24139);
#23761=SHAPE_DEFINITION_REPRESENTATION(#23877,#24140);
#23762=SHAPE_DEFINITION_REPRESENTATION(#23878,#24141);
#23763=SHAPE_DEFINITION_REPRESENTATION(#23879,#24142);
#23764=SHAPE_DEFINITION_REPRESENTATION(#23880,#24143);
#23765=SHAPE_DEFINITION_REPRESENTATION(#23881,#24144);
#23766=SHAPE_DEFINITION_REPRESENTATION(#23882,#24145);
#23767=SHAPE_DEFINITION_REPRESENTATION(#23883,#24146);
#23768=SHAPE_DEFINITION_REPRESENTATION(#23884,#24147);
#23769=SHAPE_DEFINITION_REPRESENTATION(#23885,#24148);
#23770=SHAPE_DEFINITION_REPRESENTATION(#23886,#24149);
#23771=SHAPE_DEFINITION_REPRESENTATION(#23887,#24150);
#23772=SHAPE_DEFINITION_REPRESENTATION(#23888,#24151);
#23773=SHAPE_DEFINITION_REPRESENTATION(#23889,#24152);
#23774=SHAPE_DEFINITION_REPRESENTATION(#23890,#24153);
#23775=SHAPE_DEFINITION_REPRESENTATION(#23891,#24154);
#23776=SHAPE_DEFINITION_REPRESENTATION(#23892,#24155);
#23777=SHAPE_DEFINITION_REPRESENTATION(#23893,#24156);
#23778=SHAPE_DEFINITION_REPRESENTATION(#23894,#24157);
#23779=SHAPE_DEFINITION_REPRESENTATION(#23895,#24158);
#23780=SHAPE_DEFINITION_REPRESENTATION(#23896,#24159);
#23781=SHAPE_DEFINITION_REPRESENTATION(#23897,#24160);
#23782=SHAPE_DEFINITION_REPRESENTATION(#23898,#24161);
#23783=SHAPE_DEFINITION_REPRESENTATION(#23899,#24162);
#23784=SHAPE_DEFINITION_REPRESENTATION(#23900,#24163);
#23785=SHAPE_DEFINITION_REPRESENTATION(#23901,#24164);
#23786=SHAPE_DEFINITION_REPRESENTATION(#23902,#24165);
#23787=SHAPE_DEFINITION_REPRESENTATION(#23903,#24166);
#23788=SHAPE_DEFINITION_REPRESENTATION(#23904,#24167);
#23789=SHAPE_DEFINITION_REPRESENTATION(#23905,#24168);
#23790=SHAPE_DEFINITION_REPRESENTATION(#23906,#24169);
#23791=SHAPE_DEFINITION_REPRESENTATION(#23907,#24170);
#23792=SHAPE_DEFINITION_REPRESENTATION(#23908,#24171);
#23793=SHAPE_DEFINITION_REPRESENTATION(#23909,#24172);
#23794=SHAPE_DEFINITION_REPRESENTATION(#23910,#24173);
#23795=SHAPE_DEFINITION_REPRESENTATION(#23911,#24174);
#23796=SHAPE_DEFINITION_REPRESENTATION(#23912,#24175);
#23797=SHAPE_DEFINITION_REPRESENTATION(#23913,#24176);
#23798=SHAPE_DEFINITION_REPRESENTATION(#23914,#24177);
#23799=SHAPE_DEFINITION_REPRESENTATION(#23915,#24178);
#23800=SHAPE_DEFINITION_REPRESENTATION(#23916,#24179);
#23801=SHAPE_DEFINITION_REPRESENTATION(#23917,#24180);
#23802=SHAPE_DEFINITION_REPRESENTATION(#23918,#24181);
#23803=SHAPE_DEFINITION_REPRESENTATION(#23919,#24182);
#23804=SHAPE_DEFINITION_REPRESENTATION(#23920,#24183);
#23805=SHAPE_DEFINITION_REPRESENTATION(#23921,#24184);
#23806=SHAPE_DEFINITION_REPRESENTATION(#23922,#24185);
#23807=SHAPE_DEFINITION_REPRESENTATION(#23923,#24186);
#23808=SHAPE_DEFINITION_REPRESENTATION(#23924,#24187);
#23809=SHAPE_DEFINITION_REPRESENTATION(#23925,#24188);
#23810=SHAPE_DEFINITION_REPRESENTATION(#23926,#24189);
#23811=SHAPE_DEFINITION_REPRESENTATION(#23927,#24190);
#23812=SHAPE_DEFINITION_REPRESENTATION(#23928,#24191);
#23813=SHAPE_DEFINITION_REPRESENTATION(#23929,#24192);
#23814=SHAPE_DEFINITION_REPRESENTATION(#23930,#24193);
#23815=SHAPE_DEFINITION_REPRESENTATION(#23982,#24194);
#23816=SHAPE_DEFINITION_REPRESENTATION(#23983,#24195);
#23817=SHAPE_DEFINITION_REPRESENTATION(#23984,#24196);
#23818=SHAPE_DEFINITION_REPRESENTATION(#23985,#24197);
#23819=SHAPE_DEFINITION_REPRESENTATION(#23986,#24198);
#23820=SHAPE_DEFINITION_REPRESENTATION(#23987,#24199);
#23821=SHAPE_DEFINITION_REPRESENTATION(#23988,#24200);
#23822=SHAPE_DEFINITION_REPRESENTATION(#23989,#24201);
#23823=SHAPE_DEFINITION_REPRESENTATION(#23990,#24202);
#23824=SHAPE_DEFINITION_REPRESENTATION(#23991,#24203);
#23825=SHAPE_DEFINITION_REPRESENTATION(#23992,#24204);
#23826=SHAPE_DEFINITION_REPRESENTATION(#23993,#24205);
#23827=SHAPE_DEFINITION_REPRESENTATION(#23994,#24206);
#23828=SHAPE_DEFINITION_REPRESENTATION(#23995,#24207);
#23829=SHAPE_DEFINITION_REPRESENTATION(#24067,#24208);
#23830=SHAPE_DEFINITION_REPRESENTATION(#24068,#24209);
#23831=SHAPE_DEFINITION_REPRESENTATION(#24069,#24210);
#23832=SHAPE_DEFINITION_REPRESENTATION(#24070,#24211);
#23833=SHAPE_DEFINITION_REPRESENTATION(#24071,#24212);
#23834=SHAPE_DEFINITION_REPRESENTATION(#24072,#24213);
#23835=SHAPE_DEFINITION_REPRESENTATION(#24073,#24214);
#23836=SHAPE_DEFINITION_REPRESENTATION(#24074,#24215);
#23837=SHAPE_DEFINITION_REPRESENTATION(#24075,#24216);
#23838=SHAPE_DEFINITION_REPRESENTATION(#24076,#24217);
#23839=SHAPE_DEFINITION_REPRESENTATION(#24077,#24218);
#23840=SHAPE_DEFINITION_REPRESENTATION(#24080,#24219);
#23841=SHAPE_DEFINITION_REPRESENTATION(#24091,#24220);
#23842=SHAPE_DEFINITION_REPRESENTATION(#24092,#24221);
#23843=SHAPE_DEFINITION_REPRESENTATION(#24094,#24222);
#23844=SHAPE_DEFINITION_REPRESENTATION(#24095,#24223);
#23845=SHAPE_DEFINITION_REPRESENTATION(#24096,#24224);
#23846=SHAPE_DEFINITION_REPRESENTATION(#24097,#24225);
#23847=SHAPE_DEFINITION_REPRESENTATION(#24098,#24226);
#23848=SHAPE_DEFINITION_REPRESENTATION(#24099,#24227);
#23849=PRODUCT_DEFINITION_SHAPE('',$,#24229);
#23850=PRODUCT_DEFINITION_SHAPE('',$,#24230);
#23851=PRODUCT_DEFINITION_SHAPE('',$,#24231);
#23852=PRODUCT_DEFINITION_SHAPE('',$,#24232);
#23853=PRODUCT_DEFINITION_SHAPE('',$,#24233);
#23854=PRODUCT_DEFINITION_SHAPE('',$,#24234);
#23855=PRODUCT_DEFINITION_SHAPE('',$,#24235);
#23856=PRODUCT_DEFINITION_SHAPE('',$,#24236);
#23857=PRODUCT_DEFINITION_SHAPE('',$,#24237);
#23858=PRODUCT_DEFINITION_SHAPE('',$,#24238);
#23859=PRODUCT_DEFINITION_SHAPE('',$,#24239);
#23860=PRODUCT_DEFINITION_SHAPE('',$,#24240);
#23861=PRODUCT_DEFINITION_SHAPE('',$,#24241);
#23862=PRODUCT_DEFINITION_SHAPE('',$,#24242);
#23863=PRODUCT_DEFINITION_SHAPE('',$,#24243);
#23864=PRODUCT_DEFINITION_SHAPE('',$,#24244);
#23865=PRODUCT_DEFINITION_SHAPE('',$,#24245);
#23866=PRODUCT_DEFINITION_SHAPE('',$,#24246);
#23867=PRODUCT_DEFINITION_SHAPE('',$,#24247);
#23868=PRODUCT_DEFINITION_SHAPE('',$,#24248);
#23869=PRODUCT_DEFINITION_SHAPE('',$,#24249);
#23870=PRODUCT_DEFINITION_SHAPE('',$,#24250);
#23871=PRODUCT_DEFINITION_SHAPE('',$,#24251);
#23872=PRODUCT_DEFINITION_SHAPE('',$,#24252);
#23873=PRODUCT_DEFINITION_SHAPE('',$,#24253);
#23874=PRODUCT_DEFINITION_SHAPE('',$,#24254);
#23875=PRODUCT_DEFINITION_SHAPE('',$,#24255);
#23876=PRODUCT_DEFINITION_SHAPE('',$,#24256);
#23877=PRODUCT_DEFINITION_SHAPE('',$,#24257);
#23878=PRODUCT_DEFINITION_SHAPE('',$,#24258);
#23879=PRODUCT_DEFINITION_SHAPE('',$,#24259);
#23880=PRODUCT_DEFINITION_SHAPE('',$,#24260);
#23881=PRODUCT_DEFINITION_SHAPE('',$,#24261);
#23882=PRODUCT_DEFINITION_SHAPE('',$,#24262);
#23883=PRODUCT_DEFINITION_SHAPE('',$,#24263);
#23884=PRODUCT_DEFINITION_SHAPE('',$,#24264);
#23885=PRODUCT_DEFINITION_SHAPE('',$,#24265);
#23886=PRODUCT_DEFINITION_SHAPE('',$,#24266);
#23887=PRODUCT_DEFINITION_SHAPE('',$,#24267);
#23888=PRODUCT_DEFINITION_SHAPE('',$,#24268);
#23889=PRODUCT_DEFINITION_SHAPE('',$,#24269);
#23890=PRODUCT_DEFINITION_SHAPE('',$,#24270);
#23891=PRODUCT_DEFINITION_SHAPE('',$,#24271);
#23892=PRODUCT_DEFINITION_SHAPE('',$,#24272);
#23893=PRODUCT_DEFINITION_SHAPE('',$,#24273);
#23894=PRODUCT_DEFINITION_SHAPE('',$,#24274);
#23895=PRODUCT_DEFINITION_SHAPE('',$,#24275);
#23896=PRODUCT_DEFINITION_SHAPE('',$,#24276);
#23897=PRODUCT_DEFINITION_SHAPE('',$,#24277);
#23898=PRODUCT_DEFINITION_SHAPE('',$,#24278);
#23899=PRODUCT_DEFINITION_SHAPE('',$,#24279);
#23900=PRODUCT_DEFINITION_SHAPE('',$,#24280);
#23901=PRODUCT_DEFINITION_SHAPE('',$,#24281);
#23902=PRODUCT_DEFINITION_SHAPE('',$,#24282);
#23903=PRODUCT_DEFINITION_SHAPE('',$,#24283);
#23904=PRODUCT_DEFINITION_SHAPE('',$,#24284);
#23905=PRODUCT_DEFINITION_SHAPE('',$,#24285);
#23906=PRODUCT_DEFINITION_SHAPE('',$,#24286);
#23907=PRODUCT_DEFINITION_SHAPE('',$,#24287);
#23908=PRODUCT_DEFINITION_SHAPE('',$,#24288);
#23909=PRODUCT_DEFINITION_SHAPE('',$,#24289);
#23910=PRODUCT_DEFINITION_SHAPE('',$,#24290);
#23911=PRODUCT_DEFINITION_SHAPE('',$,#24291);
#23912=PRODUCT_DEFINITION_SHAPE('',$,#24292);
#23913=PRODUCT_DEFINITION_SHAPE('',$,#24293);
#23914=PRODUCT_DEFINITION_SHAPE('',$,#24294);
#23915=PRODUCT_DEFINITION_SHAPE('',$,#24295);
#23916=PRODUCT_DEFINITION_SHAPE('',$,#24296);
#23917=PRODUCT_DEFINITION_SHAPE('',$,#24297);
#23918=PRODUCT_DEFINITION_SHAPE('',$,#24298);
#23919=PRODUCT_DEFINITION_SHAPE('',$,#24299);
#23920=PRODUCT_DEFINITION_SHAPE('',$,#24300);
#23921=PRODUCT_DEFINITION_SHAPE('',$,#24301);
#23922=PRODUCT_DEFINITION_SHAPE('',$,#24302);
#23923=PRODUCT_DEFINITION_SHAPE('',$,#24303);
#23924=PRODUCT_DEFINITION_SHAPE('',$,#24304);
#23925=PRODUCT_DEFINITION_SHAPE('',$,#24305);
#23926=PRODUCT_DEFINITION_SHAPE('',$,#24306);
#23927=PRODUCT_DEFINITION_SHAPE('',$,#24307);
#23928=PRODUCT_DEFINITION_SHAPE('',$,#24308);
#23929=PRODUCT_DEFINITION_SHAPE('',$,#24309);
#23930=PRODUCT_DEFINITION_SHAPE('',$,#24310);
#23931=PRODUCT_DEFINITION_SHAPE($,$,#452);
#23932=PRODUCT_DEFINITION_SHAPE($,$,#453);
#23933=PRODUCT_DEFINITION_SHAPE($,$,#454);
#23934=PRODUCT_DEFINITION_SHAPE($,$,#455);
#23935=PRODUCT_DEFINITION_SHAPE($,$,#456);
#23936=PRODUCT_DEFINITION_SHAPE($,$,#457);
#23937=PRODUCT_DEFINITION_SHAPE($,$,#458);
#23938=PRODUCT_DEFINITION_SHAPE($,$,#459);
#23939=PRODUCT_DEFINITION_SHAPE($,$,#460);
#23940=PRODUCT_DEFINITION_SHAPE($,$,#461);
#23941=PRODUCT_DEFINITION_SHAPE($,$,#462);
#23942=PRODUCT_DEFINITION_SHAPE($,$,#463);
#23943=PRODUCT_DEFINITION_SHAPE($,$,#464);
#23944=PRODUCT_DEFINITION_SHAPE($,$,#465);
#23945=PRODUCT_DEFINITION_SHAPE($,$,#466);
#23946=PRODUCT_DEFINITION_SHAPE($,$,#467);
#23947=PRODUCT_DEFINITION_SHAPE($,$,#468);
#23948=PRODUCT_DEFINITION_SHAPE($,$,#469);
#23949=PRODUCT_DEFINITION_SHAPE($,$,#470);
#23950=PRODUCT_DEFINITION_SHAPE($,$,#471);
#23951=PRODUCT_DEFINITION_SHAPE($,$,#472);
#23952=PRODUCT_DEFINITION_SHAPE($,$,#473);
#23953=PRODUCT_DEFINITION_SHAPE($,$,#474);
#23954=PRODUCT_DEFINITION_SHAPE($,$,#475);
#23955=PRODUCT_DEFINITION_SHAPE($,$,#476);
#23956=PRODUCT_DEFINITION_SHAPE($,$,#477);
#23957=PRODUCT_DEFINITION_SHAPE($,$,#478);
#23958=PRODUCT_DEFINITION_SHAPE($,$,#479);
#23959=PRODUCT_DEFINITION_SHAPE($,$,#480);
#23960=PRODUCT_DEFINITION_SHAPE($,$,#481);
#23961=PRODUCT_DEFINITION_SHAPE($,$,#482);
#23962=PRODUCT_DEFINITION_SHAPE($,$,#483);
#23963=PRODUCT_DEFINITION_SHAPE($,$,#484);
#23964=PRODUCT_DEFINITION_SHAPE($,$,#485);
#23965=PRODUCT_DEFINITION_SHAPE($,$,#486);
#23966=PRODUCT_DEFINITION_SHAPE($,$,#487);
#23967=PRODUCT_DEFINITION_SHAPE($,$,#488);
#23968=PRODUCT_DEFINITION_SHAPE($,$,#489);
#23969=PRODUCT_DEFINITION_SHAPE($,$,#490);
#23970=PRODUCT_DEFINITION_SHAPE($,$,#491);
#23971=PRODUCT_DEFINITION_SHAPE($,$,#492);
#23972=PRODUCT_DEFINITION_SHAPE($,$,#493);
#23973=PRODUCT_DEFINITION_SHAPE($,$,#494);
#23974=PRODUCT_DEFINITION_SHAPE($,$,#495);
#23975=PRODUCT_DEFINITION_SHAPE($,$,#496);
#23976=PRODUCT_DEFINITION_SHAPE($,$,#497);
#23977=PRODUCT_DEFINITION_SHAPE($,$,#498);
#23978=PRODUCT_DEFINITION_SHAPE($,$,#499);
#23979=PRODUCT_DEFINITION_SHAPE($,$,#500);
#23980=PRODUCT_DEFINITION_SHAPE($,$,#501);
#23981=PRODUCT_DEFINITION_SHAPE($,$,#502);
#23982=PRODUCT_DEFINITION_SHAPE('',$,#24311);
#23983=PRODUCT_DEFINITION_SHAPE('',$,#24312);
#23984=PRODUCT_DEFINITION_SHAPE('',$,#24313);
#23985=PRODUCT_DEFINITION_SHAPE('',$,#24314);
#23986=PRODUCT_DEFINITION_SHAPE('',$,#24315);
#23987=PRODUCT_DEFINITION_SHAPE('',$,#24316);
#23988=PRODUCT_DEFINITION_SHAPE('',$,#24317);
#23989=PRODUCT_DEFINITION_SHAPE('',$,#24318);
#23990=PRODUCT_DEFINITION_SHAPE('',$,#24319);
#23991=PRODUCT_DEFINITION_SHAPE('',$,#24320);
#23992=PRODUCT_DEFINITION_SHAPE('',$,#24321);
#23993=PRODUCT_DEFINITION_SHAPE('',$,#24322);
#23994=PRODUCT_DEFINITION_SHAPE('',$,#24323);
#23995=PRODUCT_DEFINITION_SHAPE('',$,#24324);
#23996=PRODUCT_DEFINITION_SHAPE($,$,#503);
#23997=PRODUCT_DEFINITION_SHAPE($,$,#504);
#23998=PRODUCT_DEFINITION_SHAPE($,$,#505);
#23999=PRODUCT_DEFINITION_SHAPE($,$,#506);
#24000=PRODUCT_DEFINITION_SHAPE($,$,#507);
#24001=PRODUCT_DEFINITION_SHAPE($,$,#508);
#24002=PRODUCT_DEFINITION_SHAPE($,$,#509);
#24003=PRODUCT_DEFINITION_SHAPE($,$,#510);
#24004=PRODUCT_DEFINITION_SHAPE($,$,#511);
#24005=PRODUCT_DEFINITION_SHAPE($,$,#512);
#24006=PRODUCT_DEFINITION_SHAPE($,$,#513);
#24007=PRODUCT_DEFINITION_SHAPE($,$,#514);
#24008=PRODUCT_DEFINITION_SHAPE($,$,#515);
#24009=PRODUCT_DEFINITION_SHAPE($,$,#516);
#24010=PRODUCT_DEFINITION_SHAPE($,$,#517);
#24011=PRODUCT_DEFINITION_SHAPE($,$,#518);
#24012=PRODUCT_DEFINITION_SHAPE($,$,#519);
#24013=PRODUCT_DEFINITION_SHAPE($,$,#520);
#24014=PRODUCT_DEFINITION_SHAPE($,$,#521);
#24015=PRODUCT_DEFINITION_SHAPE($,$,#522);
#24016=PRODUCT_DEFINITION_SHAPE($,$,#523);
#24017=PRODUCT_DEFINITION_SHAPE($,$,#524);
#24018=PRODUCT_DEFINITION_SHAPE($,$,#525);
#24019=PRODUCT_DEFINITION_SHAPE($,$,#526);
#24020=PRODUCT_DEFINITION_SHAPE($,$,#527);
#24021=PRODUCT_DEFINITION_SHAPE($,$,#528);
#24022=PRODUCT_DEFINITION_SHAPE($,$,#529);
#24023=PRODUCT_DEFINITION_SHAPE($,$,#530);
#24024=PRODUCT_DEFINITION_SHAPE($,$,#531);
#24025=PRODUCT_DEFINITION_SHAPE($,$,#532);
#24026=PRODUCT_DEFINITION_SHAPE($,$,#533);
#24027=PRODUCT_DEFINITION_SHAPE($,$,#534);
#24028=PRODUCT_DEFINITION_SHAPE($,$,#535);
#24029=PRODUCT_DEFINITION_SHAPE($,$,#536);
#24030=PRODUCT_DEFINITION_SHAPE($,$,#537);
#24031=PRODUCT_DEFINITION_SHAPE($,$,#538);
#24032=PRODUCT_DEFINITION_SHAPE($,$,#539);
#24033=PRODUCT_DEFINITION_SHAPE($,$,#540);
#24034=PRODUCT_DEFINITION_SHAPE($,$,#541);
#24035=PRODUCT_DEFINITION_SHAPE($,$,#542);
#24036=PRODUCT_DEFINITION_SHAPE($,$,#543);
#24037=PRODUCT_DEFINITION_SHAPE($,$,#544);
#24038=PRODUCT_DEFINITION_SHAPE($,$,#545);
#24039=PRODUCT_DEFINITION_SHAPE($,$,#546);
#24040=PRODUCT_DEFINITION_SHAPE($,$,#547);
#24041=PRODUCT_DEFINITION_SHAPE($,$,#548);
#24042=PRODUCT_DEFINITION_SHAPE($,$,#549);
#24043=PRODUCT_DEFINITION_SHAPE($,$,#550);
#24044=PRODUCT_DEFINITION_SHAPE($,$,#551);
#24045=PRODUCT_DEFINITION_SHAPE($,$,#552);
#24046=PRODUCT_DEFINITION_SHAPE($,$,#553);
#24047=PRODUCT_DEFINITION_SHAPE($,$,#554);
#24048=PRODUCT_DEFINITION_SHAPE($,$,#555);
#24049=PRODUCT_DEFINITION_SHAPE($,$,#556);
#24050=PRODUCT_DEFINITION_SHAPE($,$,#557);
#24051=PRODUCT_DEFINITION_SHAPE($,$,#558);
#24052=PRODUCT_DEFINITION_SHAPE($,$,#559);
#24053=PRODUCT_DEFINITION_SHAPE($,$,#560);
#24054=PRODUCT_DEFINITION_SHAPE($,$,#561);
#24055=PRODUCT_DEFINITION_SHAPE($,$,#562);
#24056=PRODUCT_DEFINITION_SHAPE($,$,#563);
#24057=PRODUCT_DEFINITION_SHAPE($,$,#564);
#24058=PRODUCT_DEFINITION_SHAPE($,$,#565);
#24059=PRODUCT_DEFINITION_SHAPE($,$,#566);
#24060=PRODUCT_DEFINITION_SHAPE($,$,#567);
#24061=PRODUCT_DEFINITION_SHAPE($,$,#568);
#24062=PRODUCT_DEFINITION_SHAPE($,$,#569);
#24063=PRODUCT_DEFINITION_SHAPE($,$,#570);
#24064=PRODUCT_DEFINITION_SHAPE($,$,#571);
#24065=PRODUCT_DEFINITION_SHAPE($,$,#572);
#24066=PRODUCT_DEFINITION_SHAPE($,$,#573);
#24067=PRODUCT_DEFINITION_SHAPE('',$,#24325);
#24068=PRODUCT_DEFINITION_SHAPE('',$,#24326);
#24069=PRODUCT_DEFINITION_SHAPE('',$,#24327);
#24070=PRODUCT_DEFINITION_SHAPE('',$,#24328);
#24071=PRODUCT_DEFINITION_SHAPE('',$,#24329);
#24072=PRODUCT_DEFINITION_SHAPE('',$,#24330);
#24073=PRODUCT_DEFINITION_SHAPE('',$,#24331);
#24074=PRODUCT_DEFINITION_SHAPE('',$,#24332);
#24075=PRODUCT_DEFINITION_SHAPE('',$,#24333);
#24076=PRODUCT_DEFINITION_SHAPE('',$,#24334);
#24077=PRODUCT_DEFINITION_SHAPE('',$,#24335);
#24078=PRODUCT_DEFINITION_SHAPE($,$,#574);
#24079=PRODUCT_DEFINITION_SHAPE($,$,#575);
#24080=PRODUCT_DEFINITION_SHAPE('',$,#24336);
#24081=PRODUCT_DEFINITION_SHAPE($,$,#576);
#24082=PRODUCT_DEFINITION_SHAPE($,$,#577);
#24083=PRODUCT_DEFINITION_SHAPE($,$,#578);
#24084=PRODUCT_DEFINITION_SHAPE($,$,#579);
#24085=PRODUCT_DEFINITION_SHAPE($,$,#580);
#24086=PRODUCT_DEFINITION_SHAPE($,$,#581);
#24087=PRODUCT_DEFINITION_SHAPE($,$,#582);
#24088=PRODUCT_DEFINITION_SHAPE($,$,#583);
#24089=PRODUCT_DEFINITION_SHAPE($,$,#584);
#24090=PRODUCT_DEFINITION_SHAPE($,$,#585);
#24091=PRODUCT_DEFINITION_SHAPE('',$,#24337);
#24092=PRODUCT_DEFINITION_SHAPE('',$,#24338);
#24093=PRODUCT_DEFINITION_SHAPE($,$,#586);
#24094=PRODUCT_DEFINITION_SHAPE('',$,#24339);
#24095=PRODUCT_DEFINITION_SHAPE('',$,#24340);
#24096=PRODUCT_DEFINITION_SHAPE('',$,#24341);
#24097=PRODUCT_DEFINITION_SHAPE('',$,#24342);
#24098=PRODUCT_DEFINITION_SHAPE('',$,#24343);
#24099=PRODUCT_DEFINITION_SHAPE('',$,#24344);
#24100=PRODUCT_DEFINITION_SHAPE($,$,#587);
#24101=PRODUCT_DEFINITION_SHAPE($,$,#588);
#24102=PRODUCT_DEFINITION_SHAPE($,$,#589);
#24103=PRODUCT_DEFINITION_SHAPE($,$,#590);
#24104=PRODUCT_DEFINITION_SHAPE($,$,#591);
#24105=PRODUCT_DEFINITION_SHAPE($,$,#592);
#24106=PRODUCT_DEFINITION_SHAPE($,$,#593);
#24107=PRODUCT_DEFINITION_SHAPE($,$,#594);
#24108=PRODUCT_DEFINITION_SHAPE($,$,#595);
#24109=PRODUCT_DEFINITION_SHAPE($,$,#596);
#24110=PRODUCT_DEFINITION_SHAPE($,$,#597);
#24111=PRODUCT_DEFINITION_SHAPE($,$,#598);
#24112=SHAPE_REPRESENTATION('',(#13676,#15467,#15468,#15469,#15470,#15471,
#15472,#15473),#23612);
#24113=SHAPE_REPRESENTATION('',(#13677,#15155,#15156,#15157,#15158,#15159,
#15160,#15161,#15162,#15163,#15164,#15165,#15166,#15167,#15168,#15169,#15170,
#15171,#15172,#15173,#15174,#15175,#15176,#15177,#15178,#15179,#15180,#15181,
#15182,#15183,#15184,#15185,#15186,#15187,#15188,#15189,#15190,#15191,#15192,
#15193,#15194,#15195,#15196,#15197,#15198,#15199,#15200,#15201,#15202,#15203,
#15204,#15205),#23613);
#24114=SHAPE_REPRESENTATION('',(#13678),#23614);
#24115=SHAPE_REPRESENTATION('',(#13721),#23615);
#24116=SHAPE_REPRESENTATION('',(#13728),#23616);
#24117=SHAPE_REPRESENTATION('',(#13735),#23617);
#24118=SHAPE_REPRESENTATION('',(#13770),#23618);
#24119=SHAPE_REPRESENTATION('',(#13805),#23619);
#24120=SHAPE_REPRESENTATION('',(#13832),#23620);
#24121=SHAPE_REPRESENTATION('',(#13841),#23621);
#24122=SHAPE_REPRESENTATION('',(#13850),#23622);
#24123=SHAPE_REPRESENTATION('',(#13859),#23623);
#24124=SHAPE_REPRESENTATION('',(#13886),#23624);
#24125=SHAPE_REPRESENTATION('',(#13895),#23625);
#24126=SHAPE_REPRESENTATION('',(#13904),#23626);
#24127=SHAPE_REPRESENTATION('',(#13913),#23627);
#24128=SHAPE_REPRESENTATION('',(#13950),#23628);
#24129=SHAPE_REPRESENTATION('',(#13974),#23629);
#24130=SHAPE_REPRESENTATION('',(#13984),#23630);
#24131=SHAPE_REPRESENTATION('',(#13994),#23631);
#24132=SHAPE_REPRESENTATION('',(#14018),#23632);
#24133=SHAPE_REPRESENTATION('',(#14028),#23633);
#24134=SHAPE_REPRESENTATION('',(#14038),#23634);
#24135=SHAPE_REPRESENTATION('',(#14075),#23635);
#24136=SHAPE_REPRESENTATION('',(#14099),#23636);
#24137=SHAPE_REPRESENTATION('',(#14109),#23637);
#24138=SHAPE_REPRESENTATION('',(#14119),#23638);
#24139=SHAPE_REPRESENTATION('',(#14143),#23639);
#24140=SHAPE_REPRESENTATION('',(#14153),#23640);
#24141=SHAPE_REPRESENTATION('',(#14163),#23641);
#24142=SHAPE_REPRESENTATION('',(#14169),#23642);
#24143=SHAPE_REPRESENTATION('',(#14175),#23643);
#24144=SHAPE_REPRESENTATION('',(#14201,#14901,#14902,#14903,#14904,#14905,
#14906,#14907,#14908,#14909,#14910,#14911,#14912,#14913,#14914,#14915,#14916,
#14917,#14918,#14919,#14920,#14921,#14922,#14923),#23644);
#24145=SHAPE_REPRESENTATION('',(#14202),#23645);
#24146=SHAPE_REPRESENTATION('',(#14243),#23646);
#24147=SHAPE_REPRESENTATION('',(#14264),#23647);
#24148=SHAPE_REPRESENTATION('',(#14274),#23648);
#24149=SHAPE_REPRESENTATION('',(#14284),#23649);
#24150=SHAPE_REPRESENTATION('',(#14294),#23650);
#24151=SHAPE_REPRESENTATION('',(#14304),#23651);
#24152=SHAPE_REPRESENTATION('',(#14325),#23652);
#24153=SHAPE_REPRESENTATION('',(#14335),#23653);
#24154=SHAPE_REPRESENTATION('',(#14345),#23654);
#24155=SHAPE_REPRESENTATION('',(#14355),#23655);
#24156=SHAPE_REPRESENTATION('',(#14365),#23656);
#24157=SHAPE_REPRESENTATION('',(#14386),#23657);
#24158=SHAPE_REPRESENTATION('',(#14396),#23658);
#24159=SHAPE_REPRESENTATION('',(#14406),#23659);
#24160=SHAPE_REPRESENTATION('',(#14416),#23660);
#24161=SHAPE_REPRESENTATION('',(#14426),#23661);
#24162=SHAPE_REPRESENTATION('',(#14447),#23662);
#24163=SHAPE_REPRESENTATION('',(#14457),#23663);
#24164=SHAPE_REPRESENTATION('',(#14467),#23664);
#24165=SHAPE_REPRESENTATION('',(#14477),#23665);
#24166=SHAPE_REPRESENTATION('',(#14487,#14924,#14925,#14926,#14927,#14928,
#14929,#14930,#14931,#14932,#14933,#14934,#14935,#14936,#14937,#14938,#14939,
#14940,#14941,#14942,#14943,#14944,#14945,#14946),#23666);
#24167=SHAPE_REPRESENTATION('',(#14488),#23667);
#24168=SHAPE_REPRESENTATION('',(#14529),#23668);
#24169=SHAPE_REPRESENTATION('',(#14550),#23669);
#24170=SHAPE_REPRESENTATION('',(#14560),#23670);
#24171=SHAPE_REPRESENTATION('',(#14570),#23671);
#24172=SHAPE_REPRESENTATION('',(#14580),#23672);
#24173=SHAPE_REPRESENTATION('',(#14590),#23673);
#24174=SHAPE_REPRESENTATION('',(#14611),#23674);
#24175=SHAPE_REPRESENTATION('',(#14621),#23675);
#24176=SHAPE_REPRESENTATION('',(#14631),#23676);
#24177=SHAPE_REPRESENTATION('',(#14641),#23677);
#24178=SHAPE_REPRESENTATION('',(#14651),#23678);
#24179=SHAPE_REPRESENTATION('',(#14672),#23679);
#24180=SHAPE_REPRESENTATION('',(#14682),#23680);
#24181=SHAPE_REPRESENTATION('',(#14692),#23681);
#24182=SHAPE_REPRESENTATION('',(#14702),#23682);
#24183=SHAPE_REPRESENTATION('',(#14712),#23683);
#24184=SHAPE_REPRESENTATION('',(#14733),#23684);
#24185=SHAPE_REPRESENTATION('',(#14743),#23685);
#24186=SHAPE_REPRESENTATION('',(#14753),#23686);
#24187=SHAPE_REPRESENTATION('',(#14763),#23687);
#24188=SHAPE_REPRESENTATION('',(#14773,#14896,#14897,#14898,#14899,#14900),
#23688);
#24189=SHAPE_REPRESENTATION('',(#14774),#23689);
#24190=SHAPE_REPRESENTATION('',(#14794),#23690);
#24191=SHAPE_REPRESENTATION('',(#14814),#23691);
#24192=SHAPE_REPRESENTATION('',(#14829),#23692);
#24193=SHAPE_REPRESENTATION('',(#14879),#23693);
#24194=SHAPE_REPRESENTATION('',(#14947,#15206,#15207,#15208,#15209,#15210,
#15211,#15212,#15213,#15214,#15215,#15216,#15217,#15218,#15219,#15220,#15221,
#15222,#15223,#15224,#15225),#23694);
#24195=SHAPE_REPRESENTATION('',(#14948),#23695);
#24196=SHAPE_REPRESENTATION('',(#14998),#23696);
#24197=SHAPE_REPRESENTATION('',(#15005),#23697);
#24198=SHAPE_REPRESENTATION('',(#15012),#23698);
#24199=SHAPE_REPRESENTATION('',(#15039),#23699);
#24200=SHAPE_REPRESENTATION('',(#15048),#23700);
#24201=SHAPE_REPRESENTATION('',(#15057),#23701);
#24202=SHAPE_REPRESENTATION('',(#15066),#23702);
#24203=SHAPE_REPRESENTATION('',(#15075),#23703);
#24204=SHAPE_REPRESENTATION('',(#15102),#23704);
#24205=SHAPE_REPRESENTATION('',(#15111),#23705);
#24206=SHAPE_REPRESENTATION('',(#15120),#23706);
#24207=SHAPE_REPRESENTATION('',(#15129),#23707);
#24208=SHAPE_REPRESENTATION('',(#15226,#15393,#15394,#15395,#15396,#15397,
#15398,#15399,#15400,#15401,#15402),#23708);
#24209=SHAPE_REPRESENTATION('',(#15227),#23709);
#24210=SHAPE_REPRESENTATION('',(#15243),#23710);
#24211=SHAPE_REPRESENTATION('',(#15259),#23711);
#24212=SHAPE_REPRESENTATION('',(#15275),#23712);
#24213=SHAPE_REPRESENTATION('',(#15285),#23713);
#24214=SHAPE_REPRESENTATION('',(#15299),#23714);
#24215=SHAPE_REPRESENTATION('',(#15308),#23715);
#24216=SHAPE_REPRESENTATION('',(#15317,#15367,#15368),#23716);
#24217=SHAPE_REPRESENTATION('',(#15318),#23717);
#24218=SHAPE_REPRESENTATION('',(#15350),#23718);
#24219=SHAPE_REPRESENTATION('',(#15369),#23719);
#24220=SHAPE_REPRESENTATION('',(#15403,#15421),#23720);
#24221=SHAPE_REPRESENTATION('',(#15404),#23721);
#24222=SHAPE_REPRESENTATION('',(#15422,#15462,#15463,#15464,#15465,#15466),
#23722);
#24223=SHAPE_REPRESENTATION('',(#15423),#23723);
#24224=SHAPE_REPRESENTATION('',(#15429),#23724);
#24225=SHAPE_REPRESENTATION('',(#15438),#23725);
#24226=SHAPE_REPRESENTATION('',(#15447),#23726);
#24227=SHAPE_REPRESENTATION('',(#15456),#23727);
#24228=PRODUCT_DEFINITION_CONTEXT('part definition',#24578,'design');
#24229=PRODUCT_DEFINITION('PAT-014','PAT-014',#24345,#24228);
#24230=PRODUCT_DEFINITION('Base and pivots','Base and pivots',#24346,#24228);
#24231=PRODUCT_DEFINITION('Base','Base',#24347,#24228);
#24232=PRODUCT_DEFINITION('Foot','Foot',#24348,#24228);
#24233=PRODUCT_DEFINITION('Foot (1)','Foot (1)',#24349,#24228);
#24234=PRODUCT_DEFINITION('Pivot post','Pivot post',#24350,#24228);
#24235=PRODUCT_DEFINITION('Pivot post (1)','Pivot post (1)',#24351,#24228);
#24236=PRODUCT_DEFINITION('Pivot pin','Pivot pin',#24352,#24228);
#24237=PRODUCT_DEFINITION('Pivot spacer 36 mm','Pivot spacer 36 mm',#24353,
#24228);
#24238=PRODUCT_DEFINITION('Pivot spacer 5 mm','Pivot spacer 5 mm',#24354,
#24228);
#24239=PRODUCT_DEFINITION('Pivot keeper','Pivot keeper',#24355,#24228);
#24240=PRODUCT_DEFINITION('Pivot pin (1)','Pivot pin (1)',#24356,#24228);
#24241=PRODUCT_DEFINITION('Pivot spacer 36 mm (1)',
'Pivot spacer 36 mm (1)',#24357,#24228);
#24242=PRODUCT_DEFINITION('Pivot spacer 5 mm (1)','Pivot spacer 5 mm (1)',
#24358,#24228);
#24243=PRODUCT_DEFINITION('Pivot keeper (1)','Pivot keeper (1)',#24359,#24228);
#24244=PRODUCT_DEFINITION('Screw and guide support',
'Screw and guide support',#24360,#24228);
#24245=PRODUCT_DEFINITION('Screw bearing keeper','Screw bearing keeper',
#24361,#24228);
#24246=PRODUCT_DEFINITION('Screw keeper fastener',
'Screw keeper fastener',#24362,#24228);
#24247=PRODUCT_DEFINITION('Screw keeper fastener (1)',
'Screw keeper fastener (1)',#24363,#24228);
#24248=PRODUCT_DEFINITION('Screw bearing keeper (1)',
'Screw bearing keeper (1)',#24364,#24228);
#24249=PRODUCT_DEFINITION('Screw keeper fastener (2)',
'Screw keeper fastener (2)',#24365,#24228);
#24250=PRODUCT_DEFINITION('Screw keeper fastener (3)',
'Screw keeper fastener (3)',#24366,#24228);
#24251=PRODUCT_DEFINITION('Screw and guide support (1)',
'Screw and guide support (1)',#24367,#24228);
#24252=PRODUCT_DEFINITION('Screw bearing keeper (2)',
'Screw bearing keeper (2)',#24368,#24228);
#24253=PRODUCT_DEFINITION('Screw keeper fastener (4)',
'Screw keeper fastener (4)',#24369,#24228);
#24254=PRODUCT_DEFINITION('Screw keeper fastener (5)',
'Screw keeper fastener (5)',#24370,#24228);
#24255=PRODUCT_DEFINITION('Screw bearing keeper (3)',
'Screw bearing keeper (3)',#24371,#24228);
#24256=PRODUCT_DEFINITION('Screw keeper fastener (6)',
'Screw keeper fastener (6)',#24372,#24228);
#24257=PRODUCT_DEFINITION('Screw keeper fastener (7)',
'Screw keeper fastener (7)',#24373,#24228);
#24258=PRODUCT_DEFINITION('Guide shaft','Guide shaft',#24374,#24228);
#24259=PRODUCT_DEFINITION('Guide shaft (1)','Guide shaft (1)',#24375,#24228);
#24260=PRODUCT_DEFINITION('Cap Screw - M5x20','Cap Screw - M5x20',#24376,
#24228);
#24261=PRODUCT_DEFINITION('Input link','Input link',#24377,#24228);
#24262=PRODUCT_DEFINITION('Input link (1)','Input link (1)',#24378,#24228);
#24263=PRODUCT_DEFINITION('Bearing cap','Bearing cap',#24379,#24228);
#24264=PRODUCT_DEFINITION('M4 short cap screw','M4 short cap screw',#24380,
#24228);
#24265=PRODUCT_DEFINITION('M4 short cap screw (1)',
'M4 short cap screw (1)',#24381,#24228);
#24266=PRODUCT_DEFINITION('M4 short cap screw (2)',
'M4 short cap screw (2)',#24382,#24228);
#24267=PRODUCT_DEFINITION('M4 short cap screw (3)',
'M4 short cap screw (3)',#24383,#24228);
#24268=PRODUCT_DEFINITION('Bearing cap (1)','Bearing cap (1)',#24384,#24228);
#24269=PRODUCT_DEFINITION('M4 short cap screw (4)',
'M4 short cap screw (4)',#24385,#24228);
#24270=PRODUCT_DEFINITION('M4 short cap screw (5)',
'M4 short cap screw (5)',#24386,#24228);
#24271=PRODUCT_DEFINITION('M4 short cap screw (6)',
'M4 short cap screw (6)',#24387,#24228);
#24272=PRODUCT_DEFINITION('M4 short cap screw (7)',
'M4 short cap screw (7)',#24388,#24228);
#24273=PRODUCT_DEFINITION('Bearing cap (2)','Bearing cap (2)',#24389,#24228);
#24274=PRODUCT_DEFINITION('M4 short cap screw (8)',
'M4 short cap screw (8)',#24390,#24228);
#24275=PRODUCT_DEFINITION('M4 short cap screw (9)',
'M4 short cap screw (9)',#24391,#24228);
#24276=PRODUCT_DEFINITION('M4 short cap screw (10)',
'M4 short cap screw (10)',#24392,#24228);
#24277=PRODUCT_DEFINITION('M4 short cap screw (11)',
'M4 short cap screw (11)',#24393,#24228);
#24278=PRODUCT_DEFINITION('Bearing cap (3)','Bearing cap (3)',#24394,#24228);
#24279=PRODUCT_DEFINITION('M4 short cap screw (12)',
'M4 short cap screw (12)',#24395,#24228);
#24280=PRODUCT_DEFINITION('M4 short cap screw (13)',
'M4 short cap screw (13)',#24396,#24228);
#24281=PRODUCT_DEFINITION('M4 short cap screw (14)',
'M4 short cap screw (14)',#24397,#24228);
#24282=PRODUCT_DEFINITION('M4 short cap screw (15)',
'M4 short cap screw (15)',#24398,#24228);
#24283=PRODUCT_DEFINITION('Output link','Output link',#24399,#24228);
#24284=PRODUCT_DEFINITION('Output link (1)','Output link (1)',#24400,#24228);
#24285=PRODUCT_DEFINITION('Bearing cap (4)','Bearing cap (4)',#24401,#24228);
#24286=PRODUCT_DEFINITION('M4 short cap screw (16)',
'M4 short cap screw (16)',#24402,#24228);
#24287=PRODUCT_DEFINITION('M4 short cap screw (17)',
'M4 short cap screw (17)',#24403,#24228);
#24288=PRODUCT_DEFINITION('M4 short cap screw (18)',
'M4 short cap screw (18)',#24404,#24228);
#24289=PRODUCT_DEFINITION('M4 short cap screw (19)',
'M4 short cap screw (19)',#24405,#24228);
#24290=PRODUCT_DEFINITION('Bearing cap (5)','Bearing cap (5)',#24406,#24228);
#24291=PRODUCT_DEFINITION('M4 short cap screw (20)',
'M4 short cap screw (20)',#24407,#24228);
#24292=PRODUCT_DEFINITION('M4 short cap screw (21)',
'M4 short cap screw (21)',#24408,#24228);
#24293=PRODUCT_DEFINITION('M4 short cap screw (22)',
'M4 short cap screw (22)',#24409,#24228);
#24294=PRODUCT_DEFINITION('M4 short cap screw (23)',
'M4 short cap screw (23)',#24410,#24228);
#24295=PRODUCT_DEFINITION('Bearing cap (6)','Bearing cap (6)',#24411,#24228);
#24296=PRODUCT_DEFINITION('M4 short cap screw (24)',
'M4 short cap screw (24)',#24412,#24228);
#24297=PRODUCT_DEFINITION('M4 short cap screw (25)',
'M4 short cap screw (25)',#24413,#24228);
#24298=PRODUCT_DEFINITION('M4 short cap screw (26)',
'M4 short cap screw (26)',#24414,#24228);
#24299=PRODUCT_DEFINITION('M4 short cap screw (27)',
'M4 short cap screw (27)',#24415,#24228);
#24300=PRODUCT_DEFINITION('Bearing cap (7)','Bearing cap (7)',#24416,#24228);
#24301=PRODUCT_DEFINITION('M4 short cap screw (28)',
'M4 short cap screw (28)',#24417,#24228);
#24302=PRODUCT_DEFINITION('M4 short cap screw (29)',
'M4 short cap screw (29)',#24418,#24228);
#24303=PRODUCT_DEFINITION('M4 short cap screw (30)',
'M4 short cap screw (30)',#24419,#24228);
#24304=PRODUCT_DEFINITION('M4 short cap screw (31)',
'M4 short cap screw (31)',#24420,#24228);
#24305=PRODUCT_DEFINITION('Sealed Ball Bearing - 12 x 32 x 10 mm',
'Sealed Ball Bearing - 12 x 32 x 10 mm',#24421,#24228);
#24306=PRODUCT_DEFINITION('Inner ring','Inner ring',#24422,#24228);
#24307=PRODUCT_DEFINITION('Outer ring','Outer ring',#24423,#24228);
#24308=PRODUCT_DEFINITION('Balls','Balls',#24424,#24228);
#24309=PRODUCT_DEFINITION('Cage','Cage',#24425,#24228);
#24310=PRODUCT_DEFINITION('Seals 2RS','Seals 2RS',#24426,#24228);
#24311=PRODUCT_DEFINITION('Tilting cradle','Tilting cradle',#24427,#24228);
#24312=PRODUCT_DEFINITION('Cradle frame','Cradle frame',#24428,#24228);
#24313=PRODUCT_DEFINITION('Cradle rim','Cradle rim',#24429,#24228);
#24314=PRODUCT_DEFINITION('Cradle rim (1)','Cradle rim (1)',#24430,#24228);
#24315=PRODUCT_DEFINITION('Actuator pivot pin','Actuator pivot pin',#24431,
#24228);
#24316=PRODUCT_DEFINITION('Pivot spacer 16 mm','Pivot spacer 16 mm',#24432,
#24228);
#24317=PRODUCT_DEFINITION('Pivot spacer 35 mm','Pivot spacer 35 mm',#24433,
#24228);
#24318=PRODUCT_DEFINITION('Pivot spacer 5 mm (2)','Pivot spacer 5 mm (2)',
#24434,#24228);
#24319=PRODUCT_DEFINITION('Pivot keeper (2)','Pivot keeper (2)',#24435,#24228);
#24320=PRODUCT_DEFINITION('Pivot pin (2)','Pivot pin (2)',#24436,#24228);
#24321=PRODUCT_DEFINITION('Pivot spacer 16 mm (1)',
'Pivot spacer 16 mm (1)',#24437,#24228);
#24322=PRODUCT_DEFINITION('Pivot spacer 5 mm (3)','Pivot spacer 5 mm (3)',
#24438,#24228);
#24323=PRODUCT_DEFINITION('Pivot keeper (3)','Pivot keeper (3)',#24439,#24228);
#24324=PRODUCT_DEFINITION('Cap Screw - M4x16','Cap Screw - M4x16',#24440,
#24228);
#24325=PRODUCT_DEFINITION('Traveling nut','Traveling nut',#24441,#24228);
#24326=PRODUCT_DEFINITION('Nut carriage','Nut carriage',#24442,#24228);
#24327=PRODUCT_DEFINITION('Guide bearing retainer',
'Guide bearing retainer',#24443,#24228);
#24328=PRODUCT_DEFINITION('Guide bearing retainer (1)',
'Guide bearing retainer (1)',#24444,#24228);
#24329=PRODUCT_DEFINITION('Connecting link clevis',
'Connecting link clevis',#24445,#24228);
#24330=PRODUCT_DEFINITION('Actuator clevis pin','Actuator clevis pin',#24446,
#24228);
#24331=PRODUCT_DEFINITION('Actuator pin keeper','Actuator pin keeper',#24447,
#24228);
#24332=PRODUCT_DEFINITION('Actuator pin spacer','Actuator pin spacer',#24448,
#24228);
#24333=PRODUCT_DEFINITION('Linear Ball Bushing - 12 x 21 x 30 mm',
'Linear Ball Bushing - 12 x 21 x 30 mm',#24449,#24228);
#24334=PRODUCT_DEFINITION('Steel sleeve','Steel sleeve',#24450,#24228);
#24335=PRODUCT_DEFINITION('Ball retainer (plastic)',
'Ball retainer (plastic)',#24451,#24228);
#24336=PRODUCT_DEFINITION('M4x10 Cap Screw','M4x10 Cap Screw',#24452,#24228);
#24337=PRODUCT_DEFINITION('Actuator connecting link',
'Actuator connecting link',#24453,#24228);
#24338=PRODUCT_DEFINITION('Actuator link','Actuator link',#24454,#24228);
#24339=PRODUCT_DEFINITION('Feed screw and handwheel',
'Feed screw and handwheel',#24455,#24228);
#24340=PRODUCT_DEFINITION('Feed screw','Feed screw',#24456,#24228);
#24341=PRODUCT_DEFINITION('Screw thrust collar','Screw thrust collar',#24457,
#24228);
#24342=PRODUCT_DEFINITION('Screw thrust collar (1)',
'Screw thrust collar (1)',#24458,#24228);
#24343=PRODUCT_DEFINITION('Handwheel','Handwheel',#24459,#24228);
#24344=PRODUCT_DEFINITION('Handwheel grip','Handwheel grip',#24460,#24228);
#24345=PRODUCT_DEFINITION_FORMATION('',$,#24580);
#24346=PRODUCT_DEFINITION_FORMATION('',$,#24581);
#24347=PRODUCT_DEFINITION_FORMATION('',$,#24582);
#24348=PRODUCT_DEFINITION_FORMATION('',$,#24583);
#24349=PRODUCT_DEFINITION_FORMATION('',$,#24584);
#24350=PRODUCT_DEFINITION_FORMATION('',$,#24585);
#24351=PRODUCT_DEFINITION_FORMATION('',$,#24586);
#24352=PRODUCT_DEFINITION_FORMATION('',$,#24587);
#24353=PRODUCT_DEFINITION_FORMATION('',$,#24588);
#24354=PRODUCT_DEFINITION_FORMATION('',$,#24589);
#24355=PRODUCT_DEFINITION_FORMATION('',$,#24590);
#24356=PRODUCT_DEFINITION_FORMATION('',$,#24591);
#24357=PRODUCT_DEFINITION_FORMATION('',$,#24592);
#24358=PRODUCT_DEFINITION_FORMATION('',$,#24593);
#24359=PRODUCT_DEFINITION_FORMATION('',$,#24594);
#24360=PRODUCT_DEFINITION_FORMATION('',$,#24595);
#24361=PRODUCT_DEFINITION_FORMATION('',$,#24596);
#24362=PRODUCT_DEFINITION_FORMATION('',$,#24597);
#24363=PRODUCT_DEFINITION_FORMATION('',$,#24598);
#24364=PRODUCT_DEFINITION_FORMATION('',$,#24599);
#24365=PRODUCT_DEFINITION_FORMATION('',$,#24600);
#24366=PRODUCT_DEFINITION_FORMATION('',$,#24601);
#24367=PRODUCT_DEFINITION_FORMATION('',$,#24602);
#24368=PRODUCT_DEFINITION_FORMATION('',$,#24603);
#24369=PRODUCT_DEFINITION_FORMATION('',$,#24604);
#24370=PRODUCT_DEFINITION_FORMATION('',$,#24605);
#24371=PRODUCT_DEFINITION_FORMATION('',$,#24606);
#24372=PRODUCT_DEFINITION_FORMATION('',$,#24607);
#24373=PRODUCT_DEFINITION_FORMATION('',$,#24608);
#24374=PRODUCT_DEFINITION_FORMATION('',$,#24609);
#24375=PRODUCT_DEFINITION_FORMATION('',$,#24610);
#24376=PRODUCT_DEFINITION_FORMATION('',$,#24611);
#24377=PRODUCT_DEFINITION_FORMATION('',$,#24612);
#24378=PRODUCT_DEFINITION_FORMATION('',$,#24613);
#24379=PRODUCT_DEFINITION_FORMATION('',$,#24614);
#24380=PRODUCT_DEFINITION_FORMATION('',$,#24615);
#24381=PRODUCT_DEFINITION_FORMATION('',$,#24616);
#24382=PRODUCT_DEFINITION_FORMATION('',$,#24617);
#24383=PRODUCT_DEFINITION_FORMATION('',$,#24618);
#24384=PRODUCT_DEFINITION_FORMATION('',$,#24619);
#24385=PRODUCT_DEFINITION_FORMATION('',$,#24620);
#24386=PRODUCT_DEFINITION_FORMATION('',$,#24621);
#24387=PRODUCT_DEFINITION_FORMATION('',$,#24622);
#24388=PRODUCT_DEFINITION_FORMATION('',$,#24623);
#24389=PRODUCT_DEFINITION_FORMATION('',$,#24624);
#24390=PRODUCT_DEFINITION_FORMATION('',$,#24625);
#24391=PRODUCT_DEFINITION_FORMATION('',$,#24626);
#24392=PRODUCT_DEFINITION_FORMATION('',$,#24627);
#24393=PRODUCT_DEFINITION_FORMATION('',$,#24628);
#24394=PRODUCT_DEFINITION_FORMATION('',$,#24629);
#24395=PRODUCT_DEFINITION_FORMATION('',$,#24630);
#24396=PRODUCT_DEFINITION_FORMATION('',$,#24631);
#24397=PRODUCT_DEFINITION_FORMATION('',$,#24632);
#24398=PRODUCT_DEFINITION_FORMATION('',$,#24633);
#24399=PRODUCT_DEFINITION_FORMATION('',$,#24634);
#24400=PRODUCT_DEFINITION_FORMATION('',$,#24635);
#24401=PRODUCT_DEFINITION_FORMATION('',$,#24636);
#24402=PRODUCT_DEFINITION_FORMATION('',$,#24637);
#24403=PRODUCT_DEFINITION_FORMATION('',$,#24638);
#24404=PRODUCT_DEFINITION_FORMATION('',$,#24639);
#24405=PRODUCT_DEFINITION_FORMATION('',$,#24640);
#24406=PRODUCT_DEFINITION_FORMATION('',$,#24641);
#24407=PRODUCT_DEFINITION_FORMATION('',$,#24642);
#24408=PRODUCT_DEFINITION_FORMATION('',$,#24643);
#24409=PRODUCT_DEFINITION_FORMATION('',$,#24644);
#24410=PRODUCT_DEFINITION_FORMATION('',$,#24645);
#24411=PRODUCT_DEFINITION_FORMATION('',$,#24646);
#24412=PRODUCT_DEFINITION_FORMATION('',$,#24647);
#24413=PRODUCT_DEFINITION_FORMATION('',$,#24648);
#24414=PRODUCT_DEFINITION_FORMATION('',$,#24649);
#24415=PRODUCT_DEFINITION_FORMATION('',$,#24650);
#24416=PRODUCT_DEFINITION_FORMATION('',$,#24651);
#24417=PRODUCT_DEFINITION_FORMATION('',$,#24652);
#24418=PRODUCT_DEFINITION_FORMATION('',$,#24653);
#24419=PRODUCT_DEFINITION_FORMATION('',$,#24654);
#24420=PRODUCT_DEFINITION_FORMATION('',$,#24655);
#24421=PRODUCT_DEFINITION_FORMATION('',$,#24656);
#24422=PRODUCT_DEFINITION_FORMATION('',$,#24657);
#24423=PRODUCT_DEFINITION_FORMATION('',$,#24658);
#24424=PRODUCT_DEFINITION_FORMATION('',$,#24659);
#24425=PRODUCT_DEFINITION_FORMATION('',$,#24660);
#24426=PRODUCT_DEFINITION_FORMATION('',$,#24661);
#24427=PRODUCT_DEFINITION_FORMATION('',$,#24662);
#24428=PRODUCT_DEFINITION_FORMATION('',$,#24663);
#24429=PRODUCT_DEFINITION_FORMATION('',$,#24664);
#24430=PRODUCT_DEFINITION_FORMATION('',$,#24665);
#24431=PRODUCT_DEFINITION_FORMATION('',$,#24666);
#24432=PRODUCT_DEFINITION_FORMATION('',$,#24667);
#24433=PRODUCT_DEFINITION_FORMATION('',$,#24668);
#24434=PRODUCT_DEFINITION_FORMATION('',$,#24669);
#24435=PRODUCT_DEFINITION_FORMATION('',$,#24670);
#24436=PRODUCT_DEFINITION_FORMATION('',$,#24671);
#24437=PRODUCT_DEFINITION_FORMATION('',$,#24672);
#24438=PRODUCT_DEFINITION_FORMATION('',$,#24673);
#24439=PRODUCT_DEFINITION_FORMATION('',$,#24674);
#24440=PRODUCT_DEFINITION_FORMATION('',$,#24675);
#24441=PRODUCT_DEFINITION_FORMATION('',$,#24676);
#24442=PRODUCT_DEFINITION_FORMATION('',$,#24677);
#24443=PRODUCT_DEFINITION_FORMATION('',$,#24678);
#24444=PRODUCT_DEFINITION_FORMATION('',$,#24679);
#24445=PRODUCT_DEFINITION_FORMATION('',$,#24680);
#24446=PRODUCT_DEFINITION_FORMATION('',$,#24681);
#24447=PRODUCT_DEFINITION_FORMATION('',$,#24682);
#24448=PRODUCT_DEFINITION_FORMATION('',$,#24683);
#24449=PRODUCT_DEFINITION_FORMATION('',$,#24684);
#24450=PRODUCT_DEFINITION_FORMATION('',$,#24685);
#24451=PRODUCT_DEFINITION_FORMATION('',$,#24686);
#24452=PRODUCT_DEFINITION_FORMATION('',$,#24687);
#24453=PRODUCT_DEFINITION_FORMATION('',$,#24688);
#24454=PRODUCT_DEFINITION_FORMATION('',$,#24689);
#24455=PRODUCT_DEFINITION_FORMATION('',$,#24690);
#24456=PRODUCT_DEFINITION_FORMATION('',$,#24691);
#24457=PRODUCT_DEFINITION_FORMATION('',$,#24692);
#24458=PRODUCT_DEFINITION_FORMATION('',$,#24693);
#24459=PRODUCT_DEFINITION_FORMATION('',$,#24694);
#24460=PRODUCT_DEFINITION_FORMATION('',$,#24695);
#24461=PRODUCT_RELATED_PRODUCT_CATEGORY('PAT-014','PAT-014',(#24580));
#24462=PRODUCT_RELATED_PRODUCT_CATEGORY('Base and pivots',
'Base and pivots',(#24581));
#24463=PRODUCT_RELATED_PRODUCT_CATEGORY('Base','Base',(#24582));
#24464=PRODUCT_RELATED_PRODUCT_CATEGORY('Foot','Foot',(#24583));
#24465=PRODUCT_RELATED_PRODUCT_CATEGORY('Foot (1)','Foot (1)',(#24584));
#24466=PRODUCT_RELATED_PRODUCT_CATEGORY('Pivot post','Pivot post',(#24585));
#24467=PRODUCT_RELATED_PRODUCT_CATEGORY('Pivot post (1)',
'Pivot post (1)',(#24586));
#24468=PRODUCT_RELATED_PRODUCT_CATEGORY('Pivot pin','Pivot pin',(#24587));
#24469=PRODUCT_RELATED_PRODUCT_CATEGORY('Pivot spacer 36 mm',
'Pivot spacer 36 mm',(#24588));
#24470=PRODUCT_RELATED_PRODUCT_CATEGORY('Pivot spacer 5 mm',
'Pivot spacer 5 mm',(#24589));
#24471=PRODUCT_RELATED_PRODUCT_CATEGORY('Pivot keeper','Pivot keeper',(#24590));
#24472=PRODUCT_RELATED_PRODUCT_CATEGORY('Pivot pin (1)','Pivot pin (1)',
(#24591));
#24473=PRODUCT_RELATED_PRODUCT_CATEGORY('Pivot spacer 36 mm (1)',
'Pivot spacer 36 mm (1)',(#24592));
#24474=PRODUCT_RELATED_PRODUCT_CATEGORY('Pivot spacer 5 mm (1)',
'Pivot spacer 5 mm (1)',(#24593));
#24475=PRODUCT_RELATED_PRODUCT_CATEGORY('Pivot keeper (1)',
'Pivot keeper (1)',(#24594));
#24476=PRODUCT_RELATED_PRODUCT_CATEGORY('Screw and guide support',
'Screw and guide support',(#24595));
#24477=PRODUCT_RELATED_PRODUCT_CATEGORY('Screw bearing keeper',
'Screw bearing keeper',(#24596));
#24478=PRODUCT_RELATED_PRODUCT_CATEGORY('Screw keeper fastener',
'Screw keeper fastener',(#24597));
#24479=PRODUCT_RELATED_PRODUCT_CATEGORY('Screw keeper fastener (1)',
'Screw keeper fastener (1)',(#24598));
#24480=PRODUCT_RELATED_PRODUCT_CATEGORY('Screw bearing keeper (1)',
'Screw bearing keeper (1)',(#24599));
#24481=PRODUCT_RELATED_PRODUCT_CATEGORY('Screw keeper fastener (2)',
'Screw keeper fastener (2)',(#24600));
#24482=PRODUCT_RELATED_PRODUCT_CATEGORY('Screw keeper fastener (3)',
'Screw keeper fastener (3)',(#24601));
#24483=PRODUCT_RELATED_PRODUCT_CATEGORY('Screw and guide support (1)',
'Screw and guide support (1)',(#24602));
#24484=PRODUCT_RELATED_PRODUCT_CATEGORY('Screw bearing keeper (2)',
'Screw bearing keeper (2)',(#24603));
#24485=PRODUCT_RELATED_PRODUCT_CATEGORY('Screw keeper fastener (4)',
'Screw keeper fastener (4)',(#24604));
#24486=PRODUCT_RELATED_PRODUCT_CATEGORY('Screw keeper fastener (5)',
'Screw keeper fastener (5)',(#24605));
#24487=PRODUCT_RELATED_PRODUCT_CATEGORY('Screw bearing keeper (3)',
'Screw bearing keeper (3)',(#24606));
#24488=PRODUCT_RELATED_PRODUCT_CATEGORY('Screw keeper fastener (6)',
'Screw keeper fastener (6)',(#24607));
#24489=PRODUCT_RELATED_PRODUCT_CATEGORY('Screw keeper fastener (7)',
'Screw keeper fastener (7)',(#24608));
#24490=PRODUCT_RELATED_PRODUCT_CATEGORY('Guide shaft','Guide shaft',(#24609));
#24491=PRODUCT_RELATED_PRODUCT_CATEGORY('Guide shaft (1)',
'Guide shaft (1)',(#24610));
#24492=PRODUCT_RELATED_PRODUCT_CATEGORY('Cap Screw - M5x20',
'Cap Screw - M5x20',(#24611));
#24493=PRODUCT_RELATED_PRODUCT_CATEGORY('Input link','Input link',(#24612));
#24494=PRODUCT_RELATED_PRODUCT_CATEGORY('Input link (1)',
'Input link (1)',(#24613));
#24495=PRODUCT_RELATED_PRODUCT_CATEGORY('Bearing cap','Bearing cap',(#24614));
#24496=PRODUCT_RELATED_PRODUCT_CATEGORY('M4 short cap screw',
'M4 short cap screw',(#24615));
#24497=PRODUCT_RELATED_PRODUCT_CATEGORY('M4 short cap screw (1)',
'M4 short cap screw (1)',(#24616));
#24498=PRODUCT_RELATED_PRODUCT_CATEGORY('M4 short cap screw (2)',
'M4 short cap screw (2)',(#24617));
#24499=PRODUCT_RELATED_PRODUCT_CATEGORY('M4 short cap screw (3)',
'M4 short cap screw (3)',(#24618));
#24500=PRODUCT_RELATED_PRODUCT_CATEGORY('Bearing cap (1)',
'Bearing cap (1)',(#24619));
#24501=PRODUCT_RELATED_PRODUCT_CATEGORY('M4 short cap screw (4)',
'M4 short cap screw (4)',(#24620));
#24502=PRODUCT_RELATED_PRODUCT_CATEGORY('M4 short cap screw (5)',
'M4 short cap screw (5)',(#24621));
#24503=PRODUCT_RELATED_PRODUCT_CATEGORY('M4 short cap screw (6)',
'M4 short cap screw (6)',(#24622));
#24504=PRODUCT_RELATED_PRODUCT_CATEGORY('M4 short cap screw (7)',
'M4 short cap screw (7)',(#24623));
#24505=PRODUCT_RELATED_PRODUCT_CATEGORY('Bearing cap (2)',
'Bearing cap (2)',(#24624));
#24506=PRODUCT_RELATED_PRODUCT_CATEGORY('M4 short cap screw (8)',
'M4 short cap screw (8)',(#24625));
#24507=PRODUCT_RELATED_PRODUCT_CATEGORY('M4 short cap screw (9)',
'M4 short cap screw (9)',(#24626));
#24508=PRODUCT_RELATED_PRODUCT_CATEGORY('M4 short cap screw (10)',
'M4 short cap screw (10)',(#24627));
#24509=PRODUCT_RELATED_PRODUCT_CATEGORY('M4 short cap screw (11)',
'M4 short cap screw (11)',(#24628));
#24510=PRODUCT_RELATED_PRODUCT_CATEGORY('Bearing cap (3)',
'Bearing cap (3)',(#24629));
#24511=PRODUCT_RELATED_PRODUCT_CATEGORY('M4 short cap screw (12)',
'M4 short cap screw (12)',(#24630));
#24512=PRODUCT_RELATED_PRODUCT_CATEGORY('M4 short cap screw (13)',
'M4 short cap screw (13)',(#24631));
#24513=PRODUCT_RELATED_PRODUCT_CATEGORY('M4 short cap screw (14)',
'M4 short cap screw (14)',(#24632));
#24514=PRODUCT_RELATED_PRODUCT_CATEGORY('M4 short cap screw (15)',
'M4 short cap screw (15)',(#24633));
#24515=PRODUCT_RELATED_PRODUCT_CATEGORY('Output link','Output link',(#24634));
#24516=PRODUCT_RELATED_PRODUCT_CATEGORY('Output link (1)',
'Output link (1)',(#24635));
#24517=PRODUCT_RELATED_PRODUCT_CATEGORY('Bearing cap (4)',
'Bearing cap (4)',(#24636));
#24518=PRODUCT_RELATED_PRODUCT_CATEGORY('M4 short cap screw (16)',
'M4 short cap screw (16)',(#24637));
#24519=PRODUCT_RELATED_PRODUCT_CATEGORY('M4 short cap screw (17)',
'M4 short cap screw (17)',(#24638));
#24520=PRODUCT_RELATED_PRODUCT_CATEGORY('M4 short cap screw (18)',
'M4 short cap screw (18)',(#24639));
#24521=PRODUCT_RELATED_PRODUCT_CATEGORY('M4 short cap screw (19)',
'M4 short cap screw (19)',(#24640));
#24522=PRODUCT_RELATED_PRODUCT_CATEGORY('Bearing cap (5)',
'Bearing cap (5)',(#24641));
#24523=PRODUCT_RELATED_PRODUCT_CATEGORY('M4 short cap screw (20)',
'M4 short cap screw (20)',(#24642));
#24524=PRODUCT_RELATED_PRODUCT_CATEGORY('M4 short cap screw (21)',
'M4 short cap screw (21)',(#24643));
#24525=PRODUCT_RELATED_PRODUCT_CATEGORY('M4 short cap screw (22)',
'M4 short cap screw (22)',(#24644));
#24526=PRODUCT_RELATED_PRODUCT_CATEGORY('M4 short cap screw (23)',
'M4 short cap screw (23)',(#24645));
#24527=PRODUCT_RELATED_PRODUCT_CATEGORY('Bearing cap (6)',
'Bearing cap (6)',(#24646));
#24528=PRODUCT_RELATED_PRODUCT_CATEGORY('M4 short cap screw (24)',
'M4 short cap screw (24)',(#24647));
#24529=PRODUCT_RELATED_PRODUCT_CATEGORY('M4 short cap screw (25)',
'M4 short cap screw (25)',(#24648));
#24530=PRODUCT_RELATED_PRODUCT_CATEGORY('M4 short cap screw (26)',
'M4 short cap screw (26)',(#24649));
#24531=PRODUCT_RELATED_PRODUCT_CATEGORY('M4 short cap screw (27)',
'M4 short cap screw (27)',(#24650));
#24532=PRODUCT_RELATED_PRODUCT_CATEGORY('Bearing cap (7)',
'Bearing cap (7)',(#24651));
#24533=PRODUCT_RELATED_PRODUCT_CATEGORY('M4 short cap screw (28)',
'M4 short cap screw (28)',(#24652));
#24534=PRODUCT_RELATED_PRODUCT_CATEGORY('M4 short cap screw (29)',
'M4 short cap screw (29)',(#24653));
#24535=PRODUCT_RELATED_PRODUCT_CATEGORY('M4 short cap screw (30)',
'M4 short cap screw (30)',(#24654));
#24536=PRODUCT_RELATED_PRODUCT_CATEGORY('M4 short cap screw (31)',
'M4 short cap screw (31)',(#24655));
#24537=PRODUCT_RELATED_PRODUCT_CATEGORY(
'Sealed Ball Bearing - 12 x 32 x 10 mm',
'Sealed Ball Bearing - 12 x 32 x 10 mm',(#24656));
#24538=PRODUCT_RELATED_PRODUCT_CATEGORY('Inner ring','Inner ring',(#24657));
#24539=PRODUCT_RELATED_PRODUCT_CATEGORY('Outer ring','Outer ring',(#24658));
#24540=PRODUCT_RELATED_PRODUCT_CATEGORY('Balls','Balls',(#24659));
#24541=PRODUCT_RELATED_PRODUCT_CATEGORY('Cage','Cage',(#24660));
#24542=PRODUCT_RELATED_PRODUCT_CATEGORY('Seals 2RS','Seals 2RS',(#24661));
#24543=PRODUCT_RELATED_PRODUCT_CATEGORY('Tilting cradle',
'Tilting cradle',(#24662));
#24544=PRODUCT_RELATED_PRODUCT_CATEGORY('Cradle frame','Cradle frame',(#24663));
#24545=PRODUCT_RELATED_PRODUCT_CATEGORY('Cradle rim','Cradle rim',(#24664));
#24546=PRODUCT_RELATED_PRODUCT_CATEGORY('Cradle rim (1)',
'Cradle rim (1)',(#24665));
#24547=PRODUCT_RELATED_PRODUCT_CATEGORY('Actuator pivot pin',
'Actuator pivot pin',(#24666));
#24548=PRODUCT_RELATED_PRODUCT_CATEGORY('Pivot spacer 16 mm',
'Pivot spacer 16 mm',(#24667));
#24549=PRODUCT_RELATED_PRODUCT_CATEGORY('Pivot spacer 35 mm',
'Pivot spacer 35 mm',(#24668));
#24550=PRODUCT_RELATED_PRODUCT_CATEGORY('Pivot spacer 5 mm (2)',
'Pivot spacer 5 mm (2)',(#24669));
#24551=PRODUCT_RELATED_PRODUCT_CATEGORY('Pivot keeper (2)',
'Pivot keeper (2)',(#24670));
#24552=PRODUCT_RELATED_PRODUCT_CATEGORY('Pivot pin (2)','Pivot pin (2)',
(#24671));
#24553=PRODUCT_RELATED_PRODUCT_CATEGORY('Pivot spacer 16 mm (1)',
'Pivot spacer 16 mm (1)',(#24672));
#24554=PRODUCT_RELATED_PRODUCT_CATEGORY('Pivot spacer 5 mm (3)',
'Pivot spacer 5 mm (3)',(#24673));
#24555=PRODUCT_RELATED_PRODUCT_CATEGORY('Pivot keeper (3)',
'Pivot keeper (3)',(#24674));
#24556=PRODUCT_RELATED_PRODUCT_CATEGORY('Cap Screw - M4x16',
'Cap Screw - M4x16',(#24675));
#24557=PRODUCT_RELATED_PRODUCT_CATEGORY('Traveling nut','Traveling nut',
(#24676));
#24558=PRODUCT_RELATED_PRODUCT_CATEGORY('Nut carriage','Nut carriage',(#24677));
#24559=PRODUCT_RELATED_PRODUCT_CATEGORY('Guide bearing retainer',
'Guide bearing retainer',(#24678));
#24560=PRODUCT_RELATED_PRODUCT_CATEGORY('Guide bearing retainer (1)',
'Guide bearing retainer (1)',(#24679));
#24561=PRODUCT_RELATED_PRODUCT_CATEGORY('Connecting link clevis',
'Connecting link clevis',(#24680));
#24562=PRODUCT_RELATED_PRODUCT_CATEGORY('Actuator clevis pin',
'Actuator clevis pin',(#24681));
#24563=PRODUCT_RELATED_PRODUCT_CATEGORY('Actuator pin keeper',
'Actuator pin keeper',(#24682));
#24564=PRODUCT_RELATED_PRODUCT_CATEGORY('Actuator pin spacer',
'Actuator pin spacer',(#24683));
#24565=PRODUCT_RELATED_PRODUCT_CATEGORY(
'Linear Ball Bushing - 12 x 21 x 30 mm',
'Linear Ball Bushing - 12 x 21 x 30 mm',(#24684));
#24566=PRODUCT_RELATED_PRODUCT_CATEGORY('Steel sleeve','Steel sleeve',(#24685));
#24567=PRODUCT_RELATED_PRODUCT_CATEGORY('Ball retainer (plastic)',
'Ball retainer (plastic)',(#24686));
#24568=PRODUCT_RELATED_PRODUCT_CATEGORY('M4x10 Cap Screw',
'M4x10 Cap Screw',(#24687));
#24569=PRODUCT_RELATED_PRODUCT_CATEGORY('Actuator connecting link',
'Actuator connecting link',(#24688));
#24570=PRODUCT_RELATED_PRODUCT_CATEGORY('Actuator link','Actuator link',
(#24689));
#24571=PRODUCT_RELATED_PRODUCT_CATEGORY('Feed screw and handwheel',
'Feed screw and handwheel',(#24690));
#24572=PRODUCT_RELATED_PRODUCT_CATEGORY('Feed screw','Feed screw',(#24691));
#24573=PRODUCT_RELATED_PRODUCT_CATEGORY('Screw thrust collar',
'Screw thrust collar',(#24692));
#24574=PRODUCT_RELATED_PRODUCT_CATEGORY('Screw thrust collar (1)',
'Screw thrust collar (1)',(#24693));
#24575=PRODUCT_RELATED_PRODUCT_CATEGORY('Handwheel','Handwheel',(#24694));
#24576=PRODUCT_RELATED_PRODUCT_CATEGORY('Handwheel grip',
'Handwheel grip',(#24695));
#24577=APPLICATION_PROTOCOL_DEFINITION('international standard',
'automotive_design',2009,#24578);
#24578=APPLICATION_CONTEXT(
'Core Data for Automotive Mechanical Design Process');
#24579=PRODUCT_CONTEXT('part definition',#24578,'mechanical');
#24580=PRODUCT('PAT-014','PAT-014','PAT-014',(#24579));
#24581=PRODUCT('Base and pivots','Base and pivots','Base and pivots',(#24579));
#24582=PRODUCT('Base','Base','Base',(#24579));
#24583=PRODUCT('Foot','Foot','Foot',(#24579));
#24584=PRODUCT('Foot (1)','Foot (1)','Foot (1)',(#24579));
#24585=PRODUCT('Pivot post','Pivot post','Pivot post',(#24579));
#24586=PRODUCT('Pivot post (1)','Pivot post (1)','Pivot post (1)',(#24579));
#24587=PRODUCT('Pivot pin','Pivot pin','Pivot pin',(#24579));
#24588=PRODUCT('Pivot spacer 36 mm','Pivot spacer 36 mm',
'Pivot spacer 36 mm',(#24579));
#24589=PRODUCT('Pivot spacer 5 mm','Pivot spacer 5 mm',
'Pivot spacer 5 mm',(#24579));
#24590=PRODUCT('Pivot keeper','Pivot keeper','Pivot keeper',(#24579));
#24591=PRODUCT('Pivot pin (1)','Pivot pin (1)','Pivot pin (1)',(#24579));
#24592=PRODUCT('Pivot spacer 36 mm (1)','Pivot spacer 36 mm (1)',
'Pivot spacer 36 mm (1)',(#24579));
#24593=PRODUCT('Pivot spacer 5 mm (1)','Pivot spacer 5 mm (1)',
'Pivot spacer 5 mm (1)',(#24579));
#24594=PRODUCT('Pivot keeper (1)','Pivot keeper (1)','Pivot keeper (1)',(#24579));
#24595=PRODUCT('Screw and guide support','Screw and guide support',
'Screw and guide support',(#24579));
#24596=PRODUCT('Screw bearing keeper','Screw bearing keeper',
'Screw bearing keeper',(#24579));
#24597=PRODUCT('Screw keeper fastener','Screw keeper fastener',
'Screw keeper fastener',(#24579));
#24598=PRODUCT('Screw keeper fastener (1)','Screw keeper fastener (1)',
'Screw keeper fastener (1)',(#24579));
#24599=PRODUCT('Screw bearing keeper (1)','Screw bearing keeper (1)',
'Screw bearing keeper (1)',(#24579));
#24600=PRODUCT('Screw keeper fastener (2)','Screw keeper fastener (2)',
'Screw keeper fastener (2)',(#24579));
#24601=PRODUCT('Screw keeper fastener (3)','Screw keeper fastener (3)',
'Screw keeper fastener (3)',(#24579));
#24602=PRODUCT('Screw and guide support (1)',
'Screw and guide support (1)','Screw and guide support (1)',(#24579));
#24603=PRODUCT('Screw bearing keeper (2)','Screw bearing keeper (2)',
'Screw bearing keeper (2)',(#24579));
#24604=PRODUCT('Screw keeper fastener (4)','Screw keeper fastener (4)',
'Screw keeper fastener (4)',(#24579));
#24605=PRODUCT('Screw keeper fastener (5)','Screw keeper fastener (5)',
'Screw keeper fastener (5)',(#24579));
#24606=PRODUCT('Screw bearing keeper (3)','Screw bearing keeper (3)',
'Screw bearing keeper (3)',(#24579));
#24607=PRODUCT('Screw keeper fastener (6)','Screw keeper fastener (6)',
'Screw keeper fastener (6)',(#24579));
#24608=PRODUCT('Screw keeper fastener (7)','Screw keeper fastener (7)',
'Screw keeper fastener (7)',(#24579));
#24609=PRODUCT('Guide shaft','Guide shaft','Guide shaft',(#24579));
#24610=PRODUCT('Guide shaft (1)','Guide shaft (1)','Guide shaft (1)',(#24579));
#24611=PRODUCT('Cap Screw - M5x20','Cap Screw - M5x20',
'Cap Screw - M5x20',(#24579));
#24612=PRODUCT('Input link','Input link','Input link',(#24579));
#24613=PRODUCT('Input link (1)','Input link (1)','Input link (1)',(#24579));
#24614=PRODUCT('Bearing cap','Bearing cap','Bearing cap',(#24579));
#24615=PRODUCT('M4 short cap screw','M4 short cap screw',
'M4 short cap screw',(#24579));
#24616=PRODUCT('M4 short cap screw (1)','M4 short cap screw (1)',
'M4 short cap screw (1)',(#24579));
#24617=PRODUCT('M4 short cap screw (2)','M4 short cap screw (2)',
'M4 short cap screw (2)',(#24579));
#24618=PRODUCT('M4 short cap screw (3)','M4 short cap screw (3)',
'M4 short cap screw (3)',(#24579));
#24619=PRODUCT('Bearing cap (1)','Bearing cap (1)','Bearing cap (1)',(#24579));
#24620=PRODUCT('M4 short cap screw (4)','M4 short cap screw (4)',
'M4 short cap screw (4)',(#24579));
#24621=PRODUCT('M4 short cap screw (5)','M4 short cap screw (5)',
'M4 short cap screw (5)',(#24579));
#24622=PRODUCT('M4 short cap screw (6)','M4 short cap screw (6)',
'M4 short cap screw (6)',(#24579));
#24623=PRODUCT('M4 short cap screw (7)','M4 short cap screw (7)',
'M4 short cap screw (7)',(#24579));
#24624=PRODUCT('Bearing cap (2)','Bearing cap (2)','Bearing cap (2)',(#24579));
#24625=PRODUCT('M4 short cap screw (8)','M4 short cap screw (8)',
'M4 short cap screw (8)',(#24579));
#24626=PRODUCT('M4 short cap screw (9)','M4 short cap screw (9)',
'M4 short cap screw (9)',(#24579));
#24627=PRODUCT('M4 short cap screw (10)','M4 short cap screw (10)',
'M4 short cap screw (10)',(#24579));
#24628=PRODUCT('M4 short cap screw (11)','M4 short cap screw (11)',
'M4 short cap screw (11)',(#24579));
#24629=PRODUCT('Bearing cap (3)','Bearing cap (3)','Bearing cap (3)',(#24579));
#24630=PRODUCT('M4 short cap screw (12)','M4 short cap screw (12)',
'M4 short cap screw (12)',(#24579));
#24631=PRODUCT('M4 short cap screw (13)','M4 short cap screw (13)',
'M4 short cap screw (13)',(#24579));
#24632=PRODUCT('M4 short cap screw (14)','M4 short cap screw (14)',
'M4 short cap screw (14)',(#24579));
#24633=PRODUCT('M4 short cap screw (15)','M4 short cap screw (15)',
'M4 short cap screw (15)',(#24579));
#24634=PRODUCT('Output link','Output link','Output link',(#24579));
#24635=PRODUCT('Output link (1)','Output link (1)','Output link (1)',(#24579));
#24636=PRODUCT('Bearing cap (4)','Bearing cap (4)','Bearing cap (4)',(#24579));
#24637=PRODUCT('M4 short cap screw (16)','M4 short cap screw (16)',
'M4 short cap screw (16)',(#24579));
#24638=PRODUCT('M4 short cap screw (17)','M4 short cap screw (17)',
'M4 short cap screw (17)',(#24579));
#24639=PRODUCT('M4 short cap screw (18)','M4 short cap screw (18)',
'M4 short cap screw (18)',(#24579));
#24640=PRODUCT('M4 short cap screw (19)','M4 short cap screw (19)',
'M4 short cap screw (19)',(#24579));
#24641=PRODUCT('Bearing cap (5)','Bearing cap (5)','Bearing cap (5)',(#24579));
#24642=PRODUCT('M4 short cap screw (20)','M4 short cap screw (20)',
'M4 short cap screw (20)',(#24579));
#24643=PRODUCT('M4 short cap screw (21)','M4 short cap screw (21)',
'M4 short cap screw (21)',(#24579));
#24644=PRODUCT('M4 short cap screw (22)','M4 short cap screw (22)',
'M4 short cap screw (22)',(#24579));
#24645=PRODUCT('M4 short cap screw (23)','M4 short cap screw (23)',
'M4 short cap screw (23)',(#24579));
#24646=PRODUCT('Bearing cap (6)','Bearing cap (6)','Bearing cap (6)',(#24579));
#24647=PRODUCT('M4 short cap screw (24)','M4 short cap screw (24)',
'M4 short cap screw (24)',(#24579));
#24648=PRODUCT('M4 short cap screw (25)','M4 short cap screw (25)',
'M4 short cap screw (25)',(#24579));
#24649=PRODUCT('M4 short cap screw (26)','M4 short cap screw (26)',
'M4 short cap screw (26)',(#24579));
#24650=PRODUCT('M4 short cap screw (27)','M4 short cap screw (27)',
'M4 short cap screw (27)',(#24579));
#24651=PRODUCT('Bearing cap (7)','Bearing cap (7)','Bearing cap (7)',(#24579));
#24652=PRODUCT('M4 short cap screw (28)','M4 short cap screw (28)',
'M4 short cap screw (28)',(#24579));
#24653=PRODUCT('M4 short cap screw (29)','M4 short cap screw (29)',
'M4 short cap screw (29)',(#24579));
#24654=PRODUCT('M4 short cap screw (30)','M4 short cap screw (30)',
'M4 short cap screw (30)',(#24579));
#24655=PRODUCT('M4 short cap screw (31)','M4 short cap screw (31)',
'M4 short cap screw (31)',(#24579));
#24656=PRODUCT('Sealed Ball Bearing - 12 x 32 x 10 mm',
'Sealed Ball Bearing - 12 x 32 x 10 mm',
'Sealed Ball Bearing - 12 x 32 x 10 mm',(#24579));
#24657=PRODUCT('Inner ring','Inner ring','Inner ring',(#24579));
#24658=PRODUCT('Outer ring','Outer ring','Outer ring',(#24579));
#24659=PRODUCT('Balls','Balls','Balls',(#24579));
#24660=PRODUCT('Cage','Cage','Cage',(#24579));
#24661=PRODUCT('Seals 2RS','Seals 2RS','Seals 2RS',(#24579));
#24662=PRODUCT('Tilting cradle','Tilting cradle','Tilting cradle',(#24579));
#24663=PRODUCT('Cradle frame','Cradle frame','Cradle frame',(#24579));
#24664=PRODUCT('Cradle rim','Cradle rim','Cradle rim',(#24579));
#24665=PRODUCT('Cradle rim (1)','Cradle rim (1)','Cradle rim (1)',(#24579));
#24666=PRODUCT('Actuator pivot pin','Actuator pivot pin',
'Actuator pivot pin',(#24579));
#24667=PRODUCT('Pivot spacer 16 mm','Pivot spacer 16 mm',
'Pivot spacer 16 mm',(#24579));
#24668=PRODUCT('Pivot spacer 35 mm','Pivot spacer 35 mm',
'Pivot spacer 35 mm',(#24579));
#24669=PRODUCT('Pivot spacer 5 mm (2)','Pivot spacer 5 mm (2)',
'Pivot spacer 5 mm (2)',(#24579));
#24670=PRODUCT('Pivot keeper (2)','Pivot keeper (2)','Pivot keeper (2)',(#24579));
#24671=PRODUCT('Pivot pin (2)','Pivot pin (2)','Pivot pin (2)',(#24579));
#24672=PRODUCT('Pivot spacer 16 mm (1)','Pivot spacer 16 mm (1)',
'Pivot spacer 16 mm (1)',(#24579));
#24673=PRODUCT('Pivot spacer 5 mm (3)','Pivot spacer 5 mm (3)',
'Pivot spacer 5 mm (3)',(#24579));
#24674=PRODUCT('Pivot keeper (3)','Pivot keeper (3)','Pivot keeper (3)',(#24579));
#24675=PRODUCT('Cap Screw - M4x16','Cap Screw - M4x16',
'Cap Screw - M4x16',(#24579));
#24676=PRODUCT('Traveling nut','Traveling nut','Traveling nut',(#24579));
#24677=PRODUCT('Nut carriage','Nut carriage','Nut carriage',(#24579));
#24678=PRODUCT('Guide bearing retainer','Guide bearing retainer',
'Guide bearing retainer',(#24579));
#24679=PRODUCT('Guide bearing retainer (1)','Guide bearing retainer (1)',
'Guide bearing retainer (1)',(#24579));
#24680=PRODUCT('Connecting link clevis','Connecting link clevis',
'Connecting link clevis',(#24579));
#24681=PRODUCT('Actuator clevis pin','Actuator clevis pin',
'Actuator clevis pin',(#24579));
#24682=PRODUCT('Actuator pin keeper','Actuator pin keeper',
'Actuator pin keeper',(#24579));
#24683=PRODUCT('Actuator pin spacer','Actuator pin spacer',
'Actuator pin spacer',(#24579));
#24684=PRODUCT('Linear Ball Bushing - 12 x 21 x 30 mm',
'Linear Ball Bushing - 12 x 21 x 30 mm',
'Linear Ball Bushing - 12 x 21 x 30 mm',(#24579));
#24685=PRODUCT('Steel sleeve','Steel sleeve','Steel sleeve',(#24579));
#24686=PRODUCT('Ball retainer (plastic)','Ball retainer (plastic)',
'Ball retainer (plastic)',(#24579));
#24687=PRODUCT('M4x10 Cap Screw','M4x10 Cap Screw','M4x10 Cap Screw',(#24579));
#24688=PRODUCT('Actuator connecting link','Actuator connecting link',
'Actuator connecting link',(#24579));
#24689=PRODUCT('Actuator link','Actuator link','Actuator link',(#24579));
#24690=PRODUCT('Feed screw and handwheel','Feed screw and handwheel',
'Feed screw and handwheel',(#24579));
#24691=PRODUCT('Feed screw','Feed screw','Feed screw',(#24579));
#24692=PRODUCT('Screw thrust collar','Screw thrust collar',
'Screw thrust collar',(#24579));
#24693=PRODUCT('Screw thrust collar (1)','Screw thrust collar (1)',
'Screw thrust collar (1)',(#24579));
#24694=PRODUCT('Handwheel','Handwheel','Handwheel',(#24579));
#24695=PRODUCT('Handwheel grip','Handwheel grip','Handwheel grip',(#24579));
#24696=PRESENTATION_STYLE_ASSIGNMENT((#24702));
#24697=PRESENTATION_STYLE_ASSIGNMENT((#24703));
#24698=PRESENTATION_STYLE_ASSIGNMENT((#24704));
#24699=PRESENTATION_STYLE_ASSIGNMENT((#24705));
#24700=PRESENTATION_STYLE_ASSIGNMENT((#24706));
#24701=PRESENTATION_STYLE_ASSIGNMENT((#24707));
#24702=SURFACE_STYLE_USAGE(.BOTH.,#24708);
#24703=SURFACE_STYLE_USAGE(.BOTH.,#24709);
#24704=SURFACE_STYLE_USAGE(.BOTH.,#24710);
#24705=SURFACE_STYLE_USAGE(.BOTH.,#24711);
#24706=SURFACE_STYLE_USAGE(.BOTH.,#24712);
#24707=SURFACE_STYLE_USAGE(.BOTH.,#24713);
#24708=SURFACE_SIDE_STYLE('',(#24714));
#24709=SURFACE_SIDE_STYLE('',(#24715));
#24710=SURFACE_SIDE_STYLE('',(#24716));
#24711=SURFACE_SIDE_STYLE('',(#24717));
#24712=SURFACE_SIDE_STYLE('',(#24718));
#24713=SURFACE_SIDE_STYLE('',(#24719));
#24714=SURFACE_STYLE_FILL_AREA(#24720);
#24715=SURFACE_STYLE_FILL_AREA(#24721);
#24716=SURFACE_STYLE_FILL_AREA(#24722);
#24717=SURFACE_STYLE_FILL_AREA(#24723);
#24718=SURFACE_STYLE_FILL_AREA(#24724);
#24719=SURFACE_STYLE_FILL_AREA(#24725);
#24720=FILL_AREA_STYLE('Steel - Satin',(#24726));
#24721=FILL_AREA_STYLE('CAD Library Painted - Deep blue',(#24727));
#24722=FILL_AREA_STYLE('CAD Library Painted - Engineering blue',(#24728));
#24723=FILL_AREA_STYLE('CAD Library Painted - Steel gray',(#24729));
#24724=FILL_AREA_STYLE('CAD Library Painted - Graphite',(#24730));
#24725=FILL_AREA_STYLE('CAD Library Painted - Light blue',(#24731));
#24726=FILL_AREA_STYLE_COLOUR('Steel - Satin',#24732);
#24727=FILL_AREA_STYLE_COLOUR('CAD Library Painted - Deep blue',#24733);
#24728=FILL_AREA_STYLE_COLOUR('CAD Library Painted - Engineering blue',
#24734);
#24729=FILL_AREA_STYLE_COLOUR('CAD Library Painted - Steel gray',#24735);
#24730=FILL_AREA_STYLE_COLOUR('CAD Library Painted - Graphite',#24736);
#24731=FILL_AREA_STYLE_COLOUR('CAD Library Painted - Light blue',#24737);
#24732=COLOUR_RGB('Steel - Satin',0.627450980392157,0.627450980392157,0.627450980392157);
#24733=COLOUR_RGB('CAD Library Painted - Deep blue',0.0784313725490196,
0.203921568627451,0.349019607843137);
#24734=COLOUR_RGB('CAD Library Painted - Engineering blue',0.12156862745098,
0.356862745098039,0.6);
#24735=COLOUR_RGB('CAD Library Painted - Steel gray',0.592156862745098,
0.631372549019608,0.67843137254902);
#24736=COLOUR_RGB('CAD Library Painted - Graphite',0.168627450980392,0.192156862745098,
0.231372549019608);
#24737=COLOUR_RGB('CAD Library Painted - Light blue',0.286274509803922,
0.552941176470588,0.780392156862745);
#24738=COLOUR_RGB('Dark Blue',0.08,0.2,0.34);
#24739=FILL_AREA_STYLE_COLOUR('',#24738);
#24740=FILL_AREA_STYLE('',(#24739));
#24741=SURFACE_STYLE_FILL_AREA(#24740);
#24742=SURFACE_SIDE_STYLE('',(#24741));
#24743=SURFACE_STYLE_USAGE(.BOTH.,#24742);
#24744=PRESENTATION_STYLE_ASSIGNMENT((#24743));
#24745=COLOUR_RGB('Light Blue',0.38,0.62,0.78);
#24746=FILL_AREA_STYLE_COLOUR('',#24745);
#24747=FILL_AREA_STYLE('',(#24746));
#24748=SURFACE_STYLE_FILL_AREA(#24747);
#24749=SURFACE_SIDE_STYLE('',(#24748));
#24750=SURFACE_STYLE_USAGE(.BOTH.,#24749);
#24751=PRESENTATION_STYLE_ASSIGNMENT((#24750));
#24752=COLOUR_RGB('Sky Blue',0.24,0.69,0.87);
#24753=FILL_AREA_STYLE_COLOUR('',#24752);
#24754=FILL_AREA_STYLE('',(#24753));
#24755=SURFACE_STYLE_FILL_AREA(#24754);
#24756=SURFACE_SIDE_STYLE('',(#24755));
#24757=SURFACE_STYLE_USAGE(.BOTH.,#24756);
#24758=PRESENTATION_STYLE_ASSIGNMENT((#24757));
#24759=COLOUR_RGB('Grey',0.48,0.52,0.57);
#24760=FILL_AREA_STYLE_COLOUR('',#24759);
#24761=FILL_AREA_STYLE('',(#24760));
#24762=SURFACE_STYLE_FILL_AREA(#24761);
#24763=SURFACE_SIDE_STYLE('',(#24762));
#24764=SURFACE_STYLE_USAGE(.BOTH.,#24763);
#24765=PRESENTATION_STYLE_ASSIGNMENT((#24764));
#24766=COLOUR_RGB('Black',0.12,0.14,0.17);
#24767=FILL_AREA_STYLE_COLOUR('',#24766);
#24768=FILL_AREA_STYLE('',(#24767));
#24769=SURFACE_STYLE_FILL_AREA(#24768);
#24770=SURFACE_SIDE_STYLE('',(#24769));
#24771=SURFACE_STYLE_USAGE(.BOTH.,#24770);
#24772=PRESENTATION_STYLE_ASSIGNMENT((#24771));
#24773=COLOUR_RGB('Off White',0.89,0.88,0.83);
#24774=FILL_AREA_STYLE_COLOUR('',#24773);
#24775=FILL_AREA_STYLE('',(#24774));
#24776=SURFACE_STYLE_FILL_AREA(#24775);
#24777=SURFACE_SIDE_STYLE('',(#24776));
#24778=SURFACE_STYLE_USAGE(.BOTH.,#24777);
#24779=PRESENTATION_STYLE_ASSIGNMENT((#24778));
ENDSEC;
END-ISO-10303-21;
